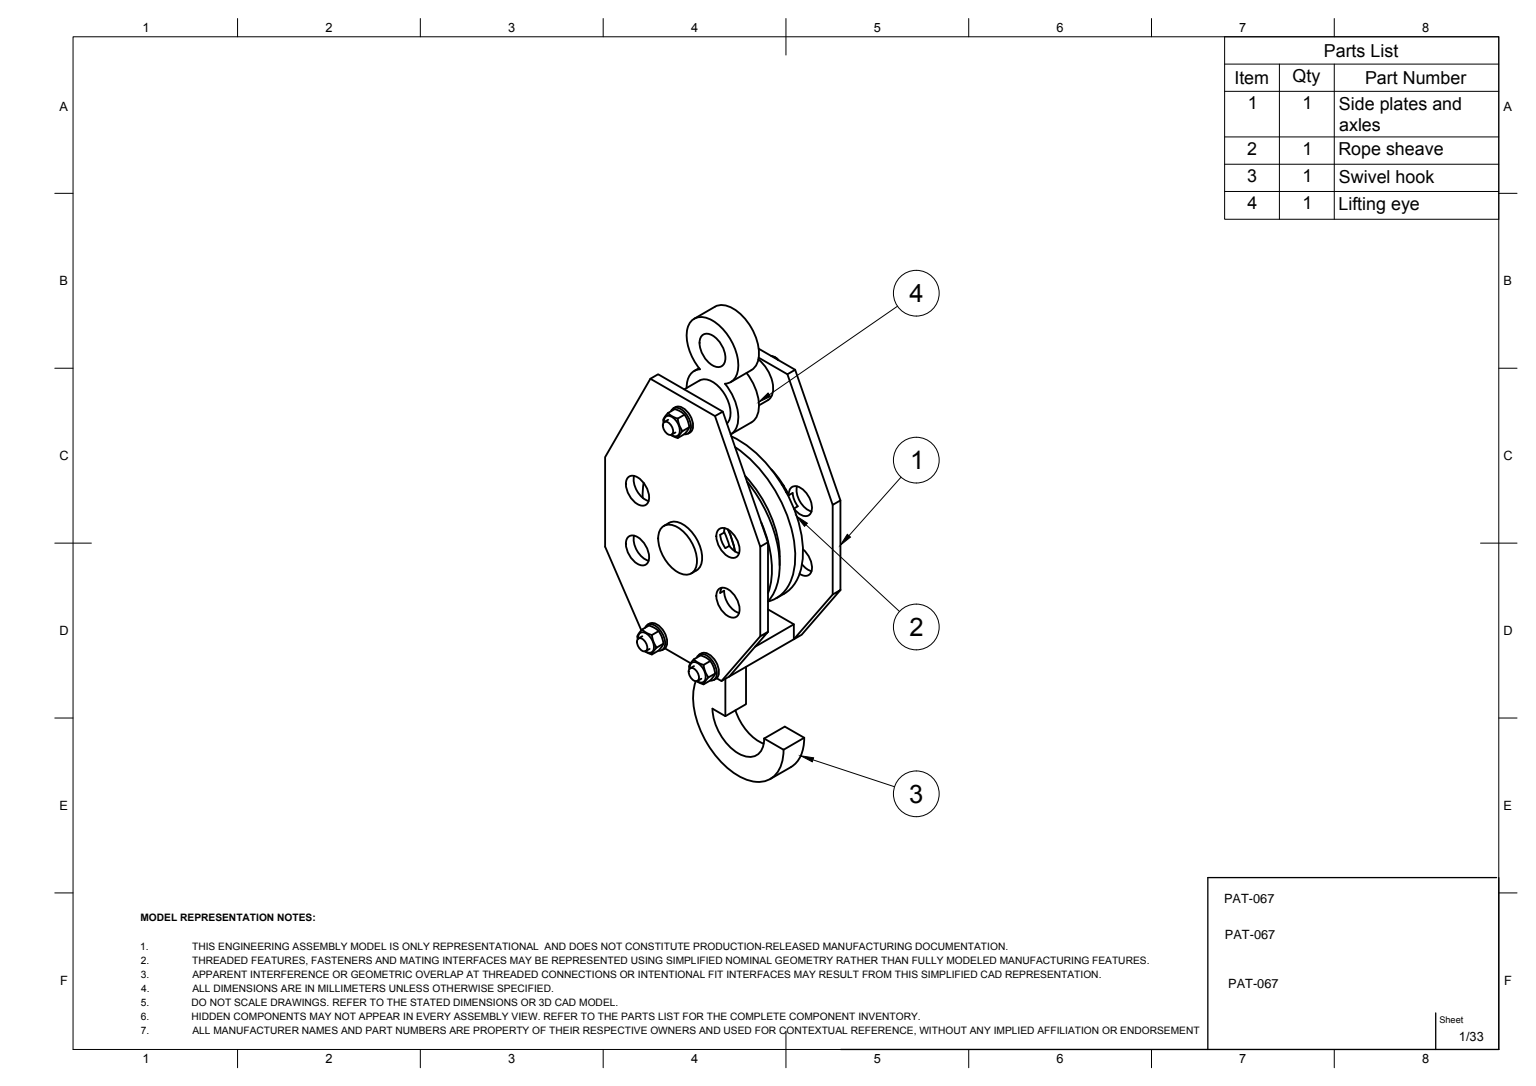
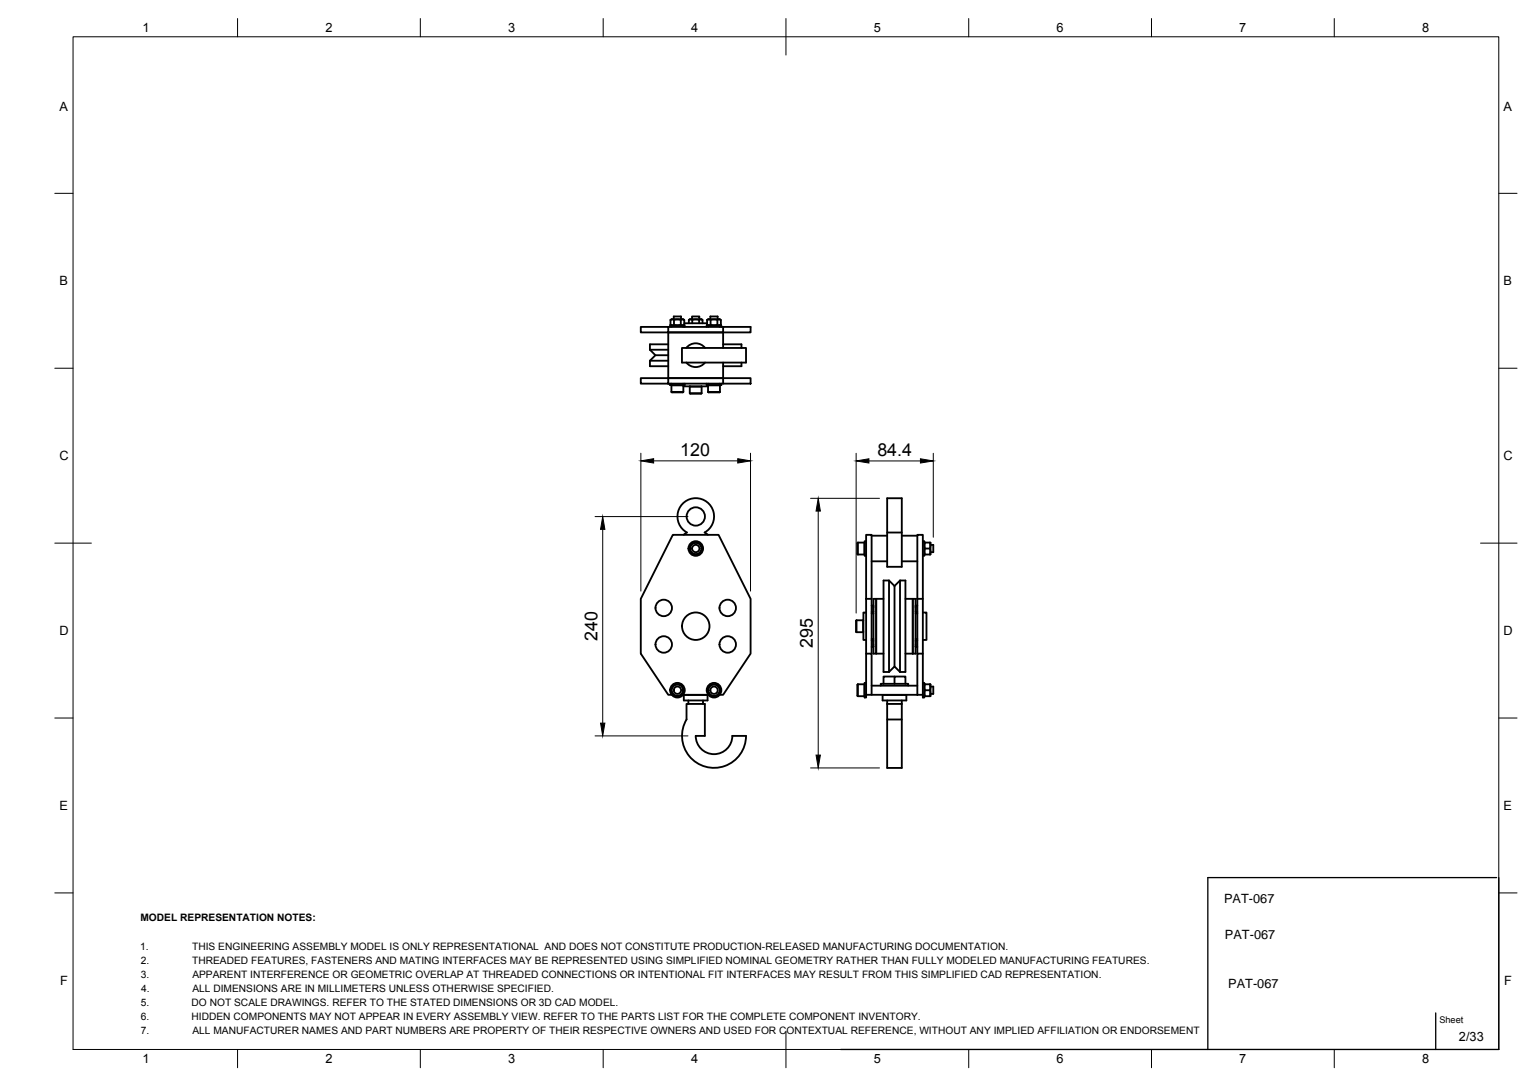
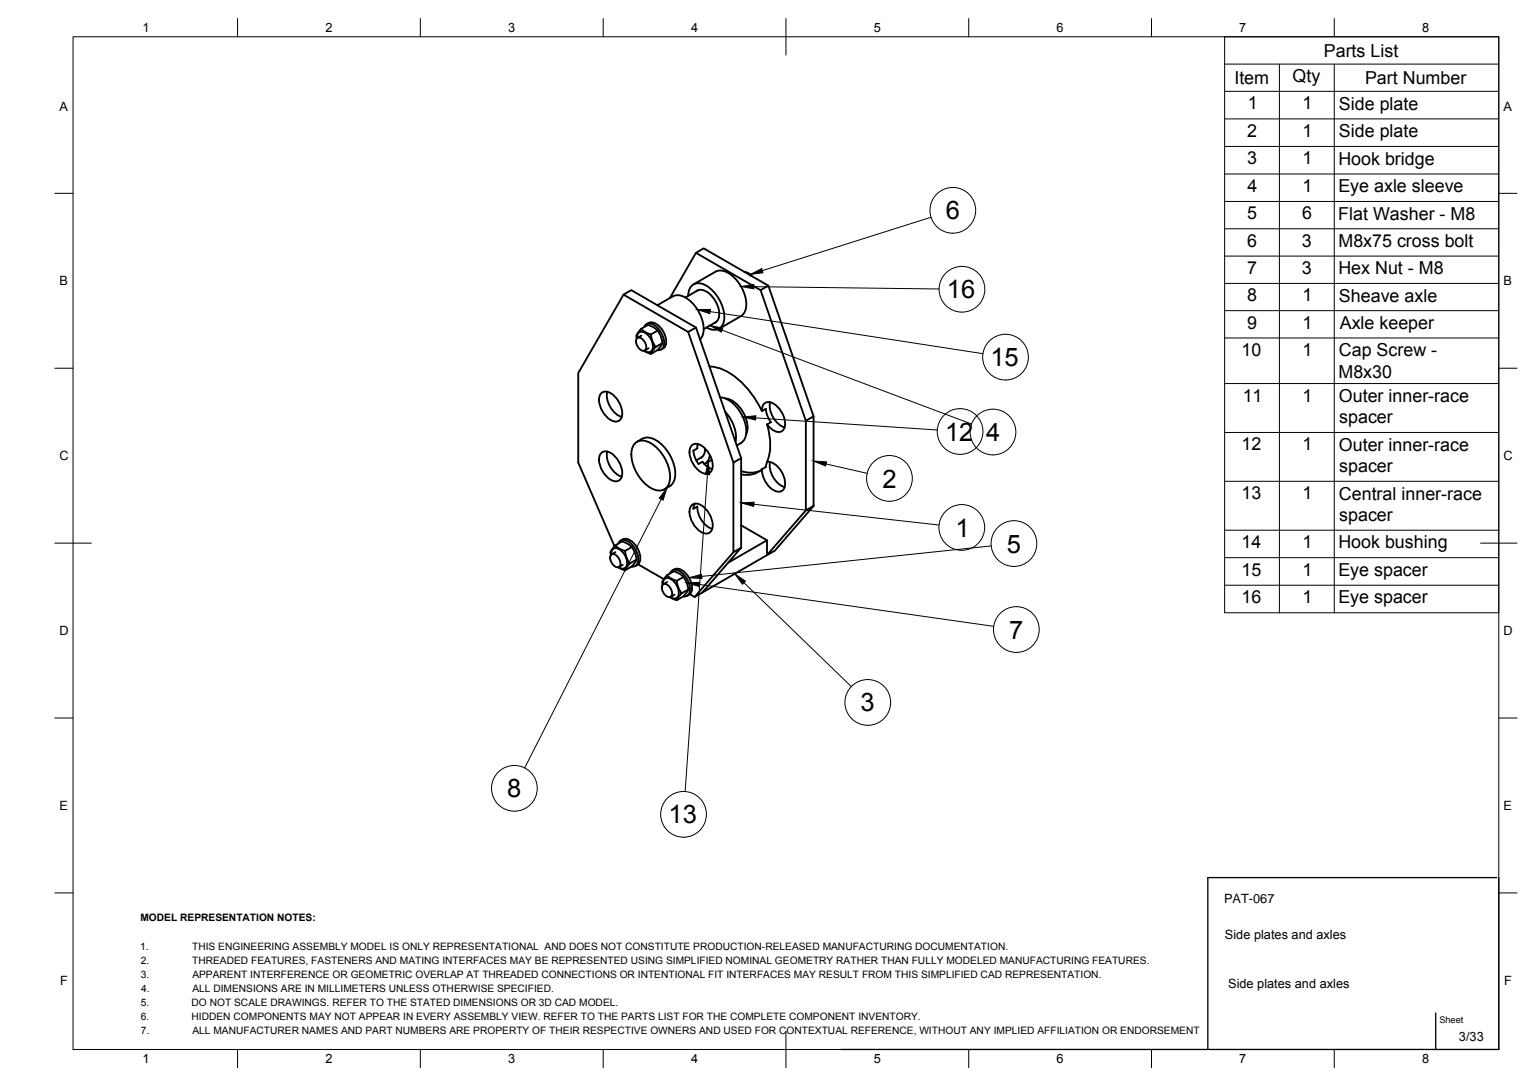
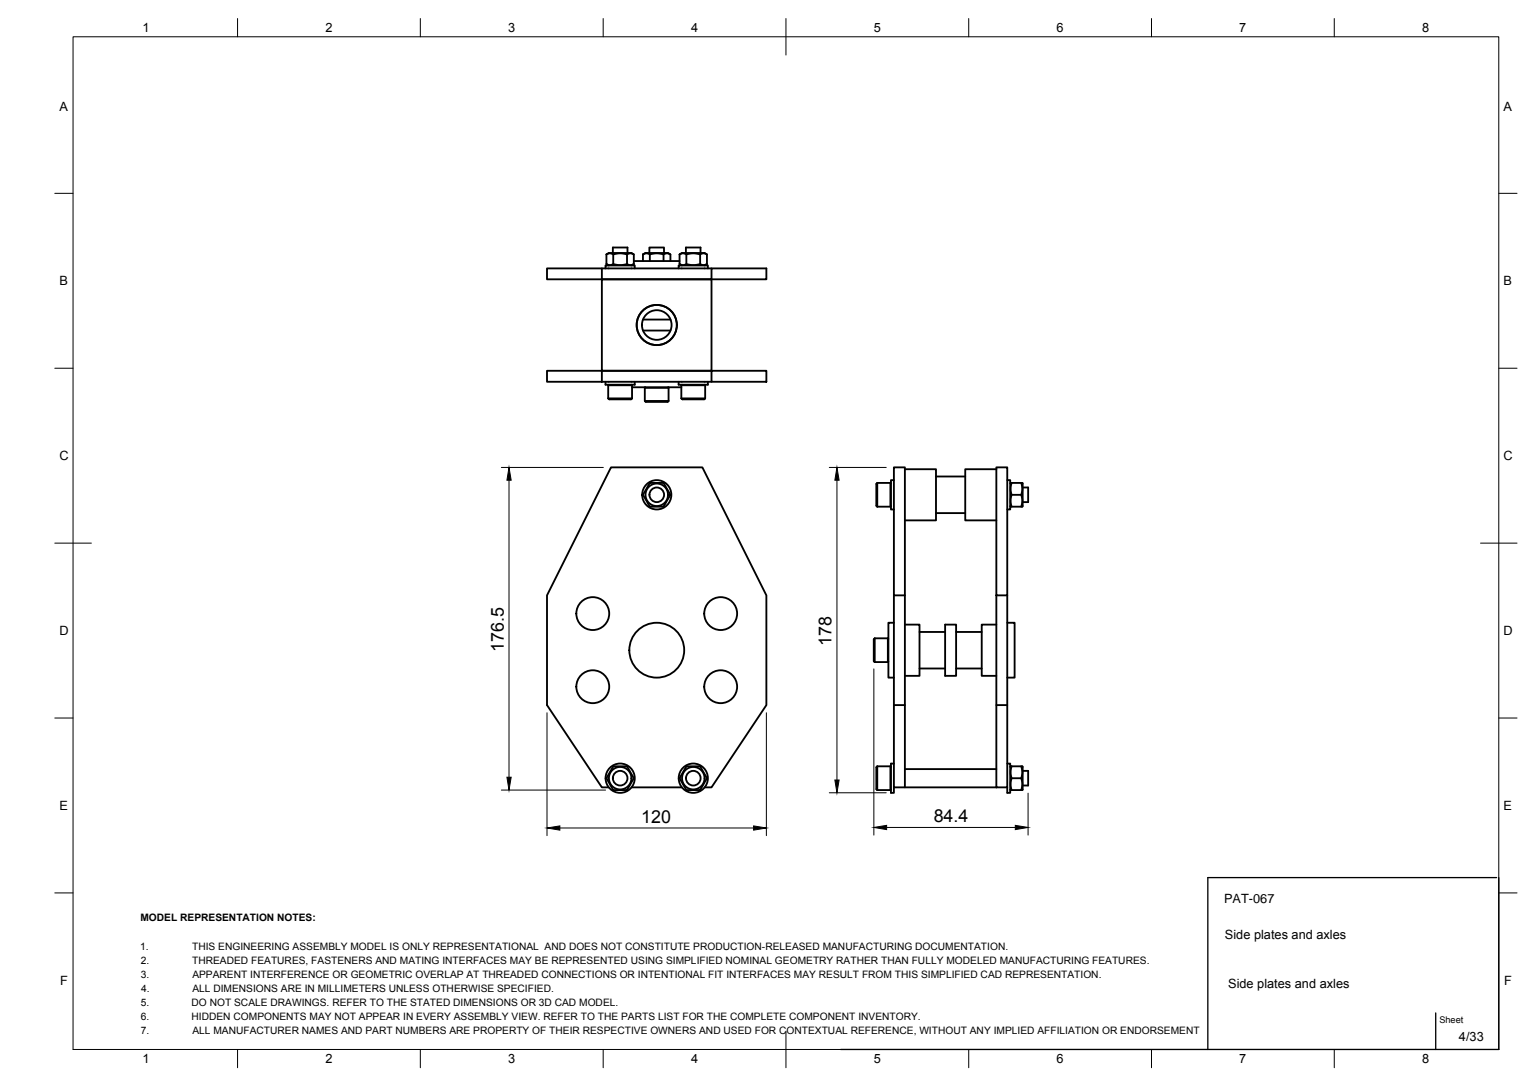
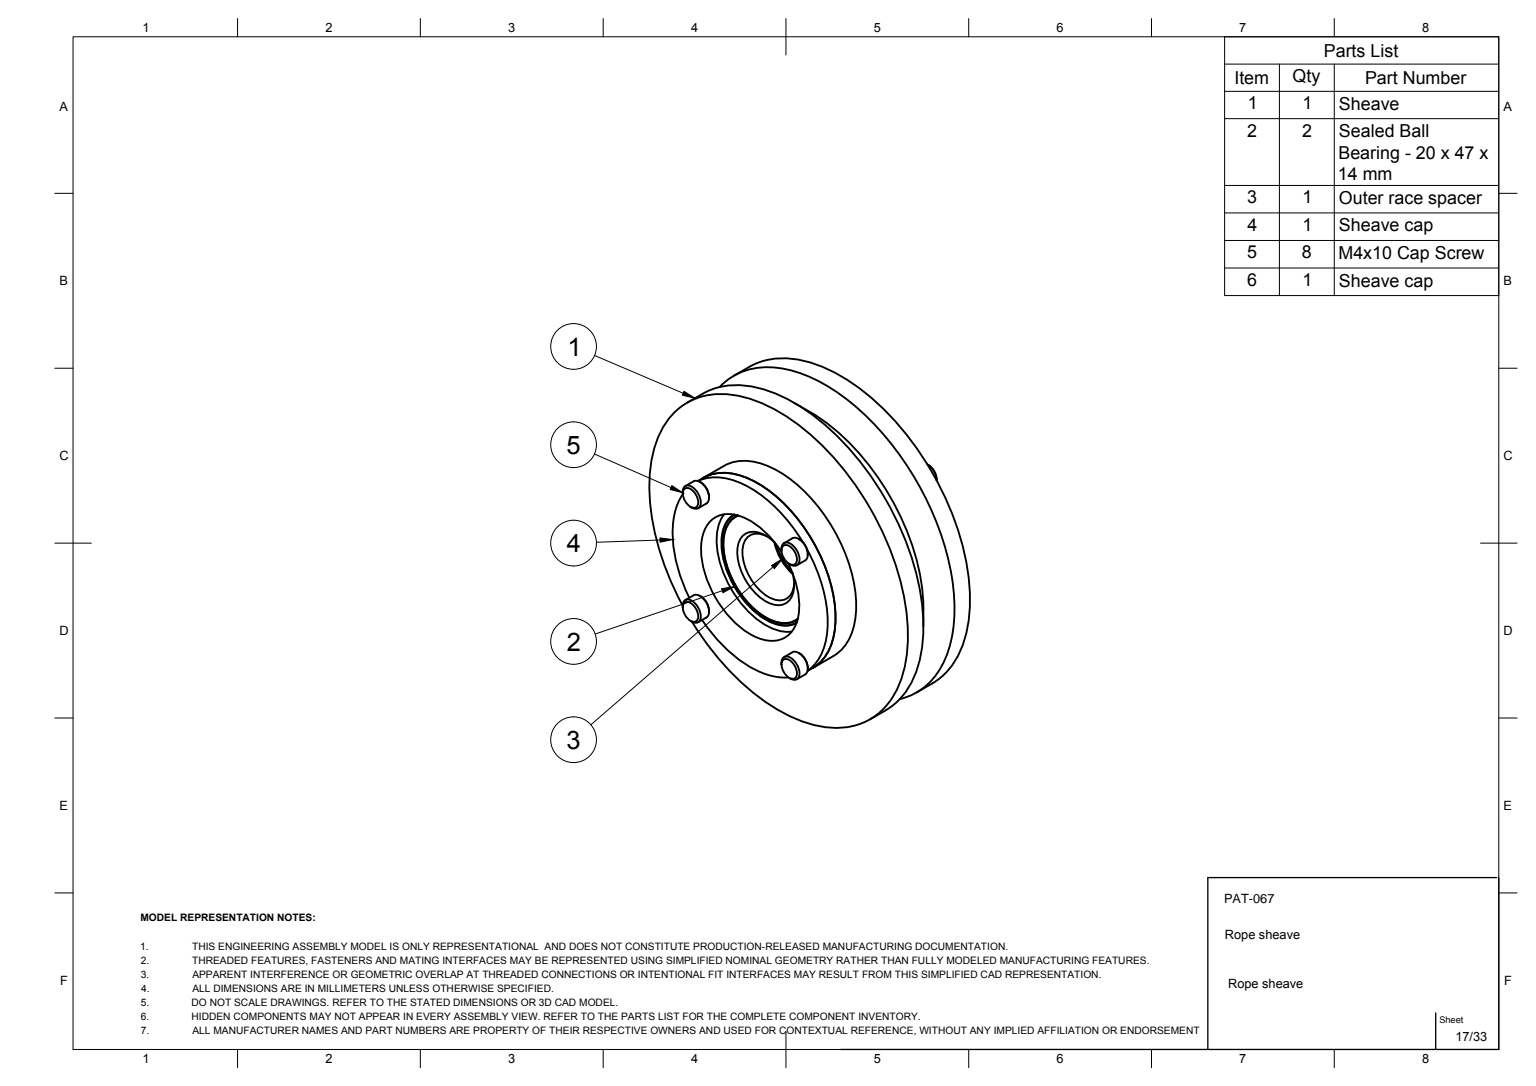
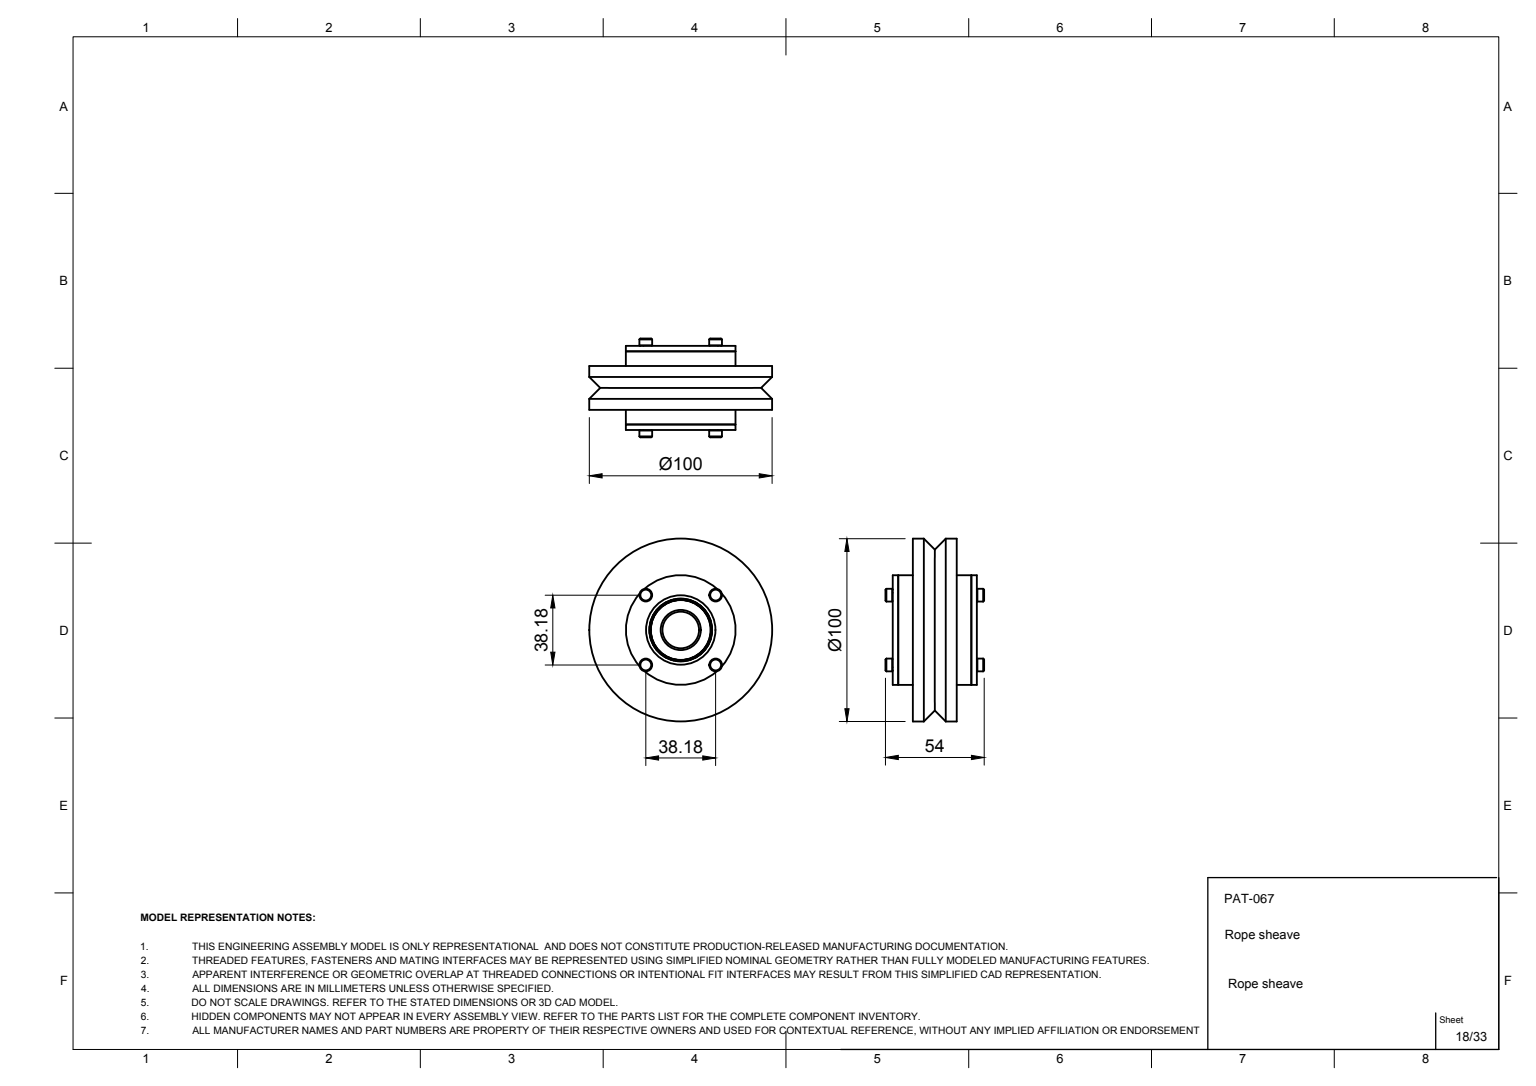
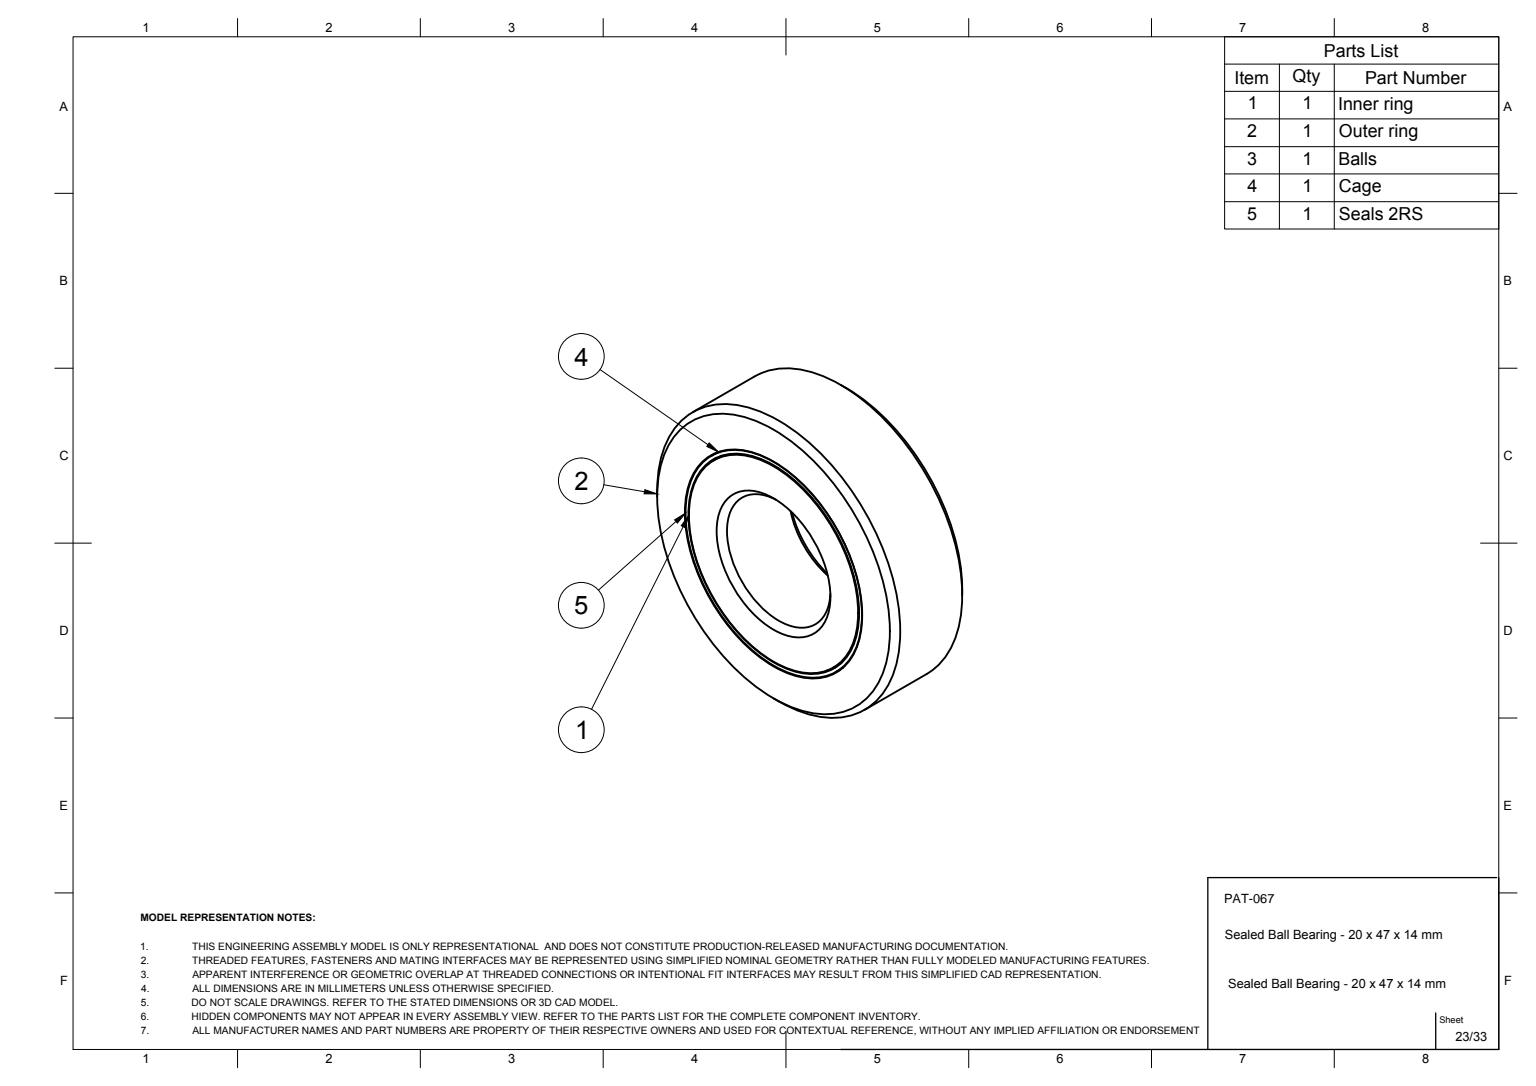
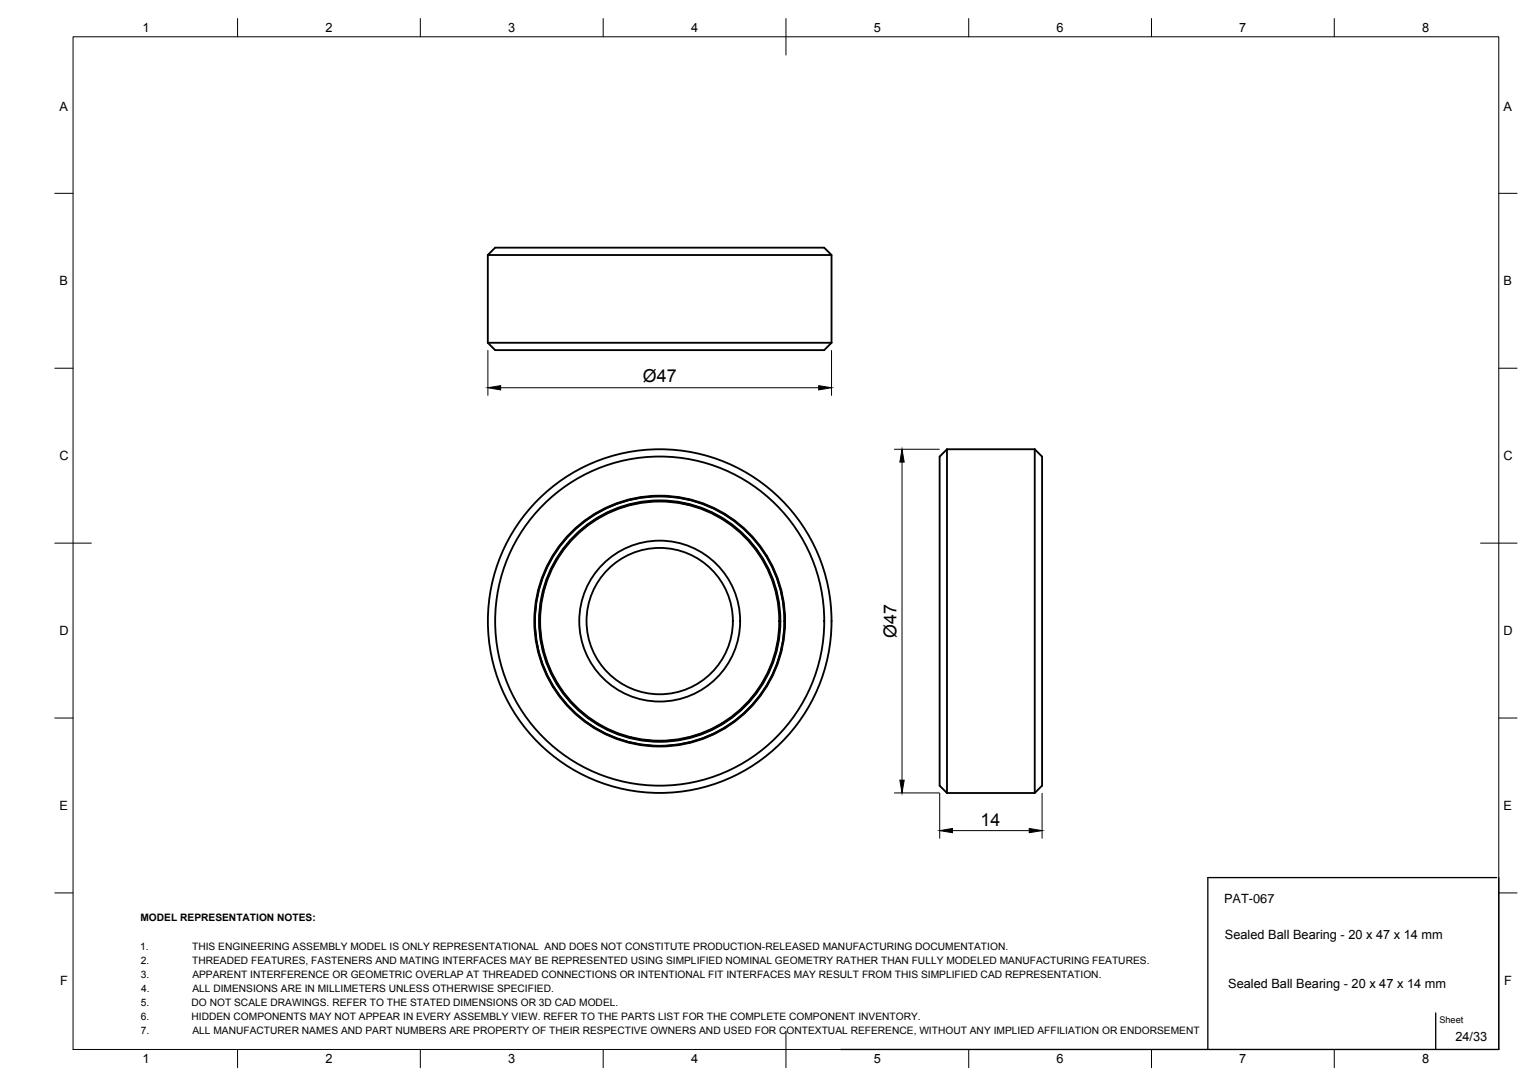
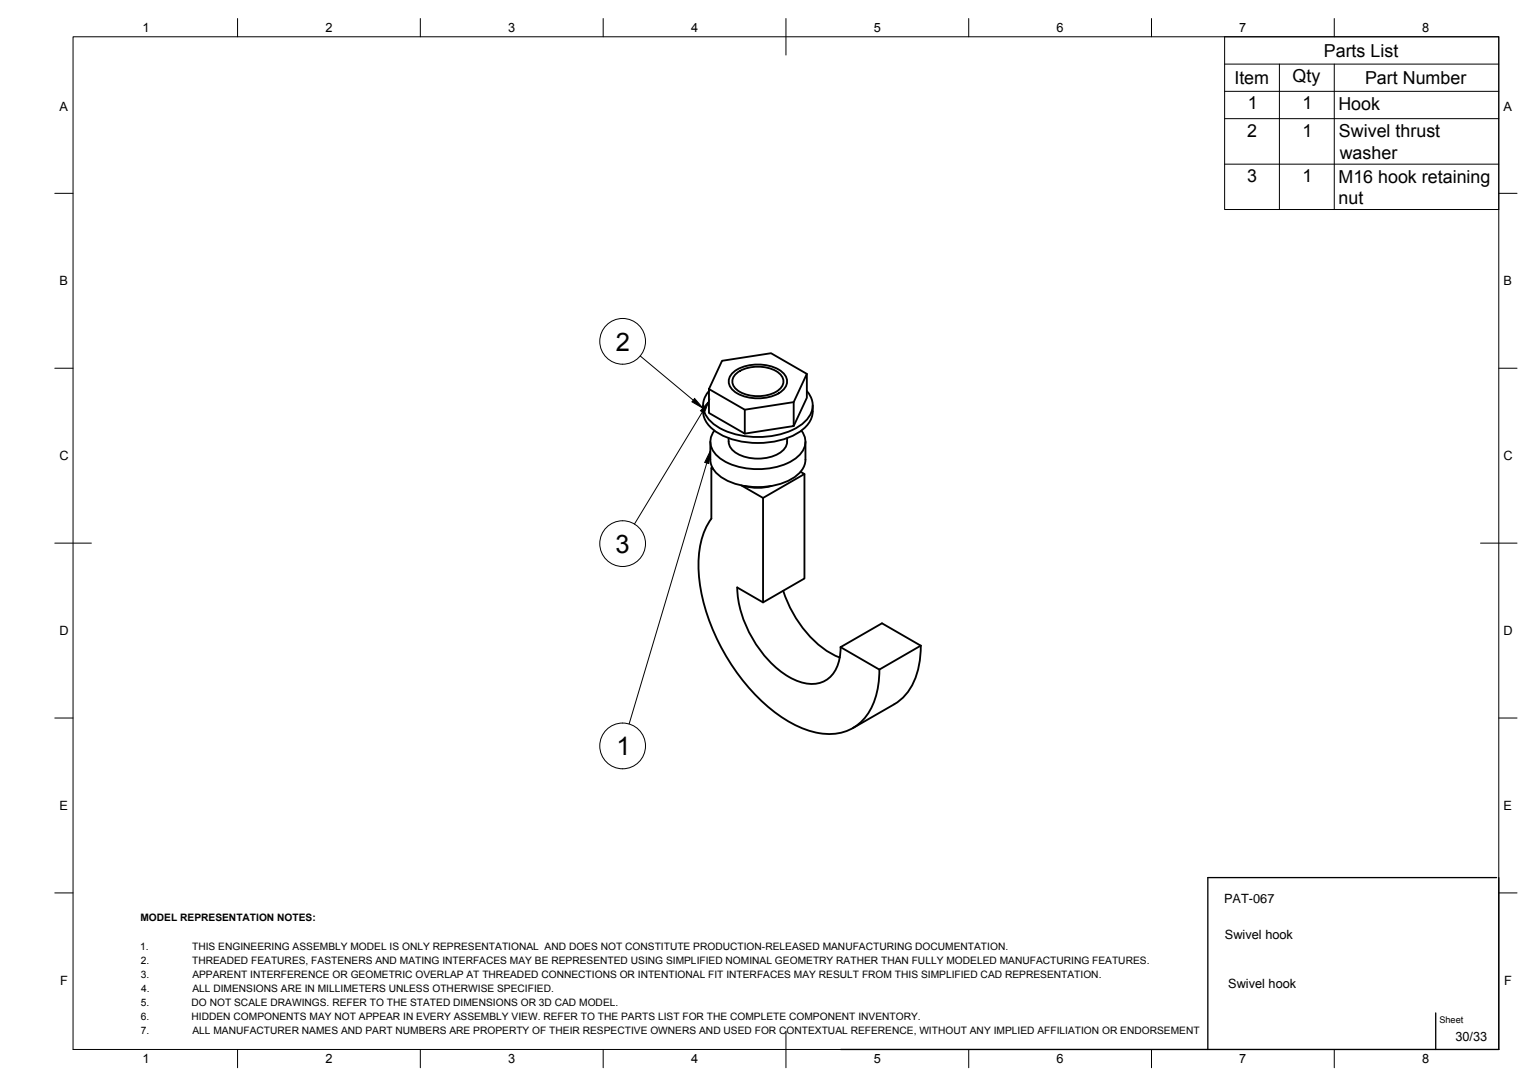
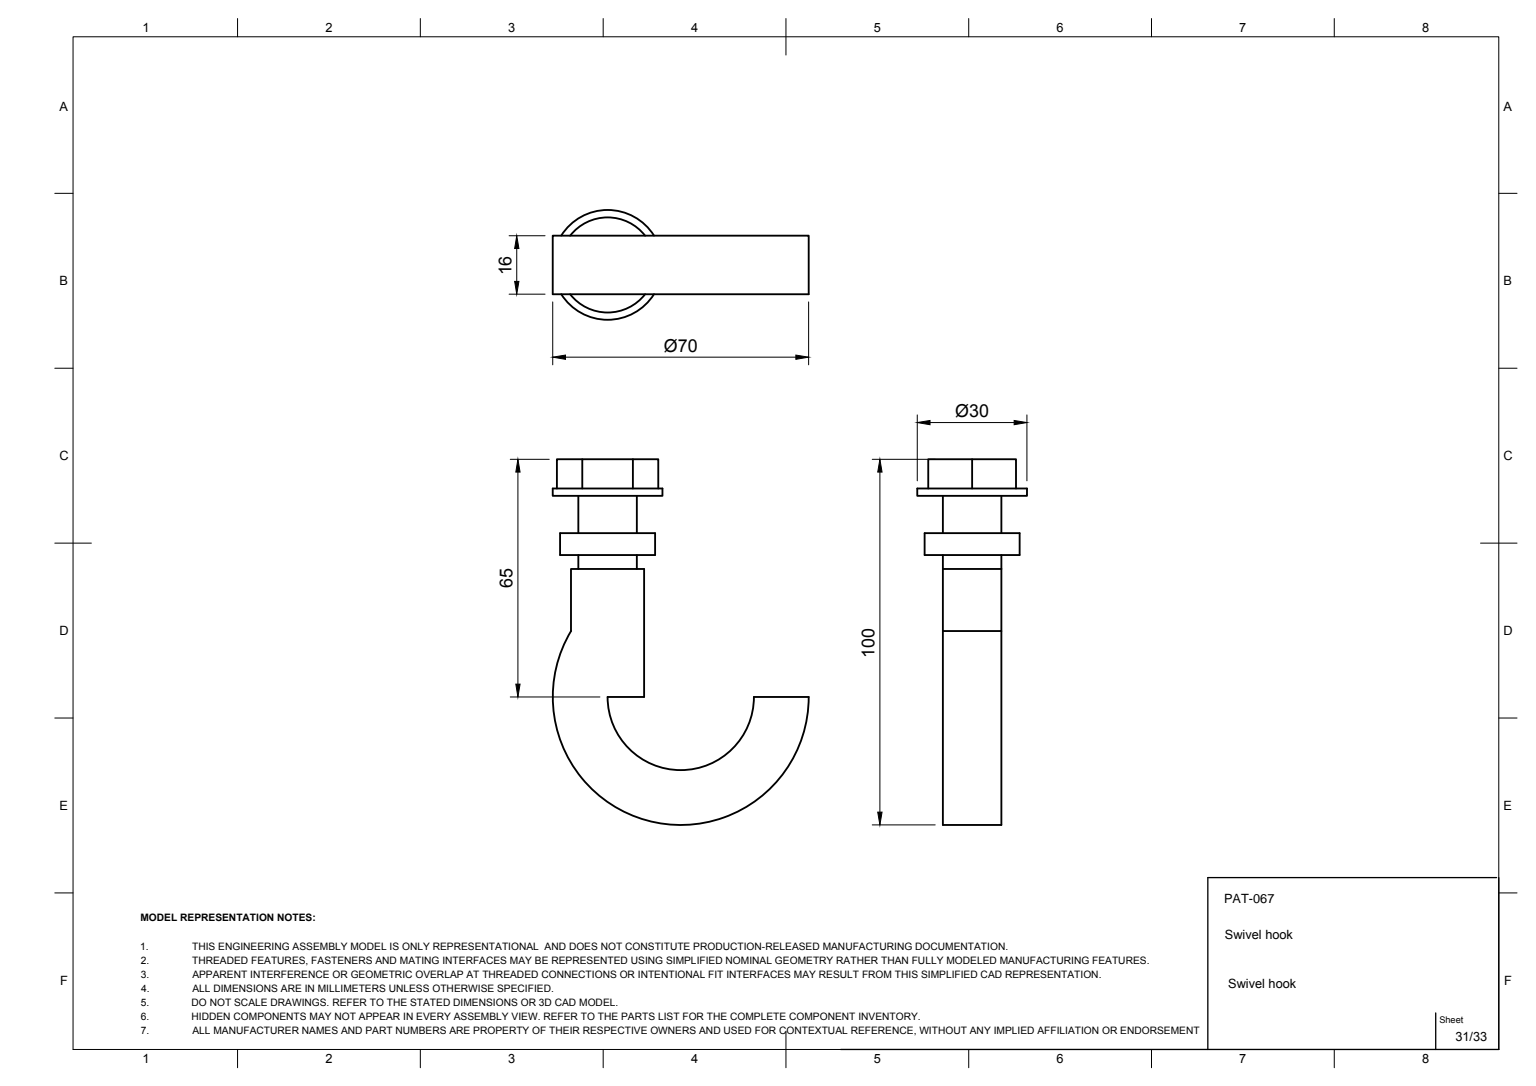
ISO-10303-21;
HEADER;
/* Generated by software containing ST-Developer
 * from STEP Tools, Inc. (www.steptools.com) 
 */

FILE_DESCRIPTION(
/* description */ ('Lifting hook block with sheave'),
/* implementation_level */ '2;1');

FILE_NAME(
/* name */ 'PAT-067',
/* time_stamp */ '2026-10-28T03:23:54-07:00',
/* author */ (''),
/* organization */ (''),
/* preprocessor_version */ 'ST-DEVELOPER v20.2',
/* originating_system */ 'Autodesk Translation Framework v15.17.0.0',
/* authorisation */ '');

FILE_SCHEMA (('AUTOMOTIVE_DESIGN { 1 0 10303 214 3 1 1 }'));
ENDSEC;

DATA;
#10=MECHANICAL_DESIGN_GEOMETRIC_PRESENTATION_REPRESENTATION('',(#351,#352,
#353,#354,#355,#356,#357,#358,#359,#360,#361,#362,#363,#364,#365,#366,#367,
#368,#369,#370,#371,#372,#373,#374,#375,#376,#377,#378,#379,#380,#381,#382,
#383,#384,#385,#386,#387,#388),#9391);
#11=B_SPLINE_CURVE_WITH_KNOTS('',3,(#8590,#8591,#8592,#8593,#8594,#8595,
#8596,#8597,#8598,#8599,#8600,#8601,#8602,#8603,#8604,#8605,#8606,#8607,
#8608,#8609,#8610,#8611),.UNSPECIFIED.,.F.,.F.,(4,2,2,2,2,2,2,2,2,2,4),
(0.0789094028588958,0.210573405340968,0.315860108011452,0.421146810681936,
0.522142632548711,0.623138454415485,0.72413427628226,0.825130098149035,
0.930416800819519,1.03570350349,1.16736750597208),.UNSPECIFIED.);
#12=B_SPLINE_CURVE_WITH_KNOTS('',3,(#8615,#8616,#8617,#8618,#8619,#8620,
#8621,#8622,#8623,#8624,#8625,#8626,#8627,#8628,#8629,#8630,#8631,#8632,
#8633,#8634,#8635,#8636),.UNSPECIFIED.,.F.,.F.,(4,2,2,2,2,2,2,2,2,2,4),
(0.0774793363974613,0.142088896491891,0.284177792983782,0.411119756996526,
0.514392970548519,0.617666184100513,0.720939397652506,0.8242126112045,0.951154575217244,
1.09324347170913,1.15785303180356),.UNSPECIFIED.);
#13=B_SPLINE_CURVE_WITH_KNOTS('',3,(#8642,#8643,#8644,#8645,#8646,#8647,
#8648,#8649,#8650,#8651,#8652,#8653,#8654,#8655,#8656,#8657,#8658,#8659,
#8660,#8661,#8662,#8663),.UNSPECIFIED.,.F.,.F.,(4,2,2,2,2,2,2,2,2,2,4),
(0.0774793363974613,0.142088896491891,0.284177792983782,0.411119756996525,
0.514392970548519,0.617666184100513,0.720939397652506,0.8242126112045,0.951154575217243,
1.09324347170913,1.15785303180356),.UNSPECIFIED.);
#14=B_SPLINE_CURVE_WITH_KNOTS('',3,(#8667,#8668,#8669,#8670,#8671,#8672,
#8673,#8674,#8675,#8676,#8677,#8678,#8679,#8680,#8681,#8682,#8683,#8684,
#8685,#8686,#8687,#8688),.UNSPECIFIED.,.F.,.F.,(4,2,2,2,2,2,2,2,2,2,4),
(0.0774793363974614,0.142088896491891,0.284177792983781,0.411119756996525,
0.514392970548519,0.617666184100512,0.720939397652506,0.824212611204499,
0.951154575217243,1.09324347170913,1.15785303180356),.UNSPECIFIED.);
#15=B_SPLINE_CURVE_WITH_KNOTS('',3,(#8692,#8693,#8694,#8695,#8696,#8697,
#8698,#8699,#8700,#8701,#8702,#8703),.UNSPECIFIED.,.F.,.F.,(4,2,2,2,2,4),
(0.0774793363974613,0.142088896491891,0.284177792983781,0.411119756996525,
0.514392970548519,0.617666184100512),.UNSPECIFIED.);
#16=B_SPLINE_CURVE_WITH_KNOTS('',3,(#8708,#8709,#8710,#8711,#8712,#8713,
#8714,#8715,#8716,#8717,#8718,#8719),.UNSPECIFIED.,.F.,.F.,(4,2,2,2,2,4),
(0.617666184100512,0.720939397652506,0.824212611204499,0.951154575217243,
1.09324347170913,1.15785303180356),.UNSPECIFIED.);
#17=B_SPLINE_CURVE_WITH_KNOTS('',3,(#8723,#8724,#8725,#8726,#8727,#8728,
#8729,#8730,#8731,#8732,#8733,#8734,#8735,#8736,#8737,#8738,#8739,#8740,
#8741,#8742,#8743,#8744),.UNSPECIFIED.,.F.,.F.,(4,2,2,2,2,2,2,2,2,2,4),
(0.0774793363974613,0.142088896491891,0.284177792983782,0.411119756996526,
0.514392970548519,0.617666184100513,0.720939397652507,0.8242126112045,0.951154575217245,
1.09324347170914,1.15785303180356),.UNSPECIFIED.);
#18=B_SPLINE_CURVE_WITH_KNOTS('',3,(#8748,#8749,#8750,#8751,#8752,#8753,
#8754,#8755,#8756,#8757,#8758,#8759,#8760,#8761,#8762,#8763,#8764,#8765,
#8766,#8767,#8768,#8769),.UNSPECIFIED.,.F.,.F.,(4,2,2,2,2,2,2,2,2,2,4),
(0.0774793363974613,0.142088896491891,0.284177792983782,0.411119756996526,
0.514392970548519,0.617666184100513,0.720939397652506,0.824212611204499,
0.951154575217243,1.09324347170913,1.15785303180356),.UNSPECIFIED.);
#19=B_SPLINE_CURVE_WITH_KNOTS('',3,(#8773,#8774,#8775,#8776,#8777,#8778,
#8779,#8780,#8781,#8782,#8783,#8784,#8785,#8786,#8787,#8788,#8789,#8790,
#8791,#8792,#8793,#8794),.UNSPECIFIED.,.F.,.F.,(4,2,2,2,2,2,2,2,2,2,4),
(0.0774793363974613,0.142088896491891,0.284177792983782,0.411119756996526,
0.514392970548519,0.617666184100513,0.720939397652506,0.8242126112045,0.951154575217244,
1.09324347170913,1.15785303180356),.UNSPECIFIED.);
#20=B_SPLINE_CURVE_WITH_KNOTS('',3,(#8798,#8799,#8800,#8801,#8802,#8803,
#8804,#8805,#8806,#8807,#8808,#8809,#8810,#8811,#8812,#8813,#8814,#8815,
#8816,#8817,#8818,#8819),.UNSPECIFIED.,.F.,.F.,(4,2,2,2,2,2,2,2,2,2,4),
(0.0774793363974613,0.142088896491891,0.284177792983782,0.411119756996526,
0.514392970548519,0.617666184100513,0.720939397652506,0.8242126112045,0.951154575217243,
1.09324347170913,1.15785303180356),.UNSPECIFIED.);
#21=B_SPLINE_CURVE_WITH_KNOTS('',3,(#8827,#8828,#8829,#8830,#8831,#8832,
#8833,#8834,#8835,#8836,#8837,#8838,#8839,#8840,#8841,#8842,#8843,#8844,
#8845,#8846,#8847,#8848),.UNSPECIFIED.,.F.,.F.,(4,2,2,2,2,2,2,2,2,2,4),
(0.0789094028588958,0.210573405340968,0.315860108011452,0.421146810681936,
0.522142632548711,0.623138454415485,0.72413427628226,0.825130098149035,
0.930416800819519,1.03570350349,1.16736750597208),.UNSPECIFIED.);
#22=B_SPLINE_CURVE_WITH_KNOTS('',3,(#8856,#8857,#8858,#8859,#8860,#8861,
#8862,#8863,#8864,#8865,#8866,#8867,#8868,#8869,#8870,#8871,#8872,#8873,
#8874,#8875,#8876,#8877),.UNSPECIFIED.,.F.,.F.,(4,2,2,2,2,2,2,2,2,2,4),
(0.0789094028588958,0.210573405340969,0.315860108011453,0.421146810681937,
0.522142632548712,0.623138454415486,0.724134276282261,0.825130098149035,
0.930416800819519,1.03570350349,1.16736750597208),.UNSPECIFIED.);
#23=B_SPLINE_CURVE_WITH_KNOTS('',3,(#8886,#8887,#8888,#8889,#8890,#8891,
#8892,#8893,#8894,#8895,#8896,#8897),.UNSPECIFIED.,.F.,.F.,(4,2,2,2,2,4),
(0.0789094028588958,0.210573405340968,0.315860108011452,0.421146810681937,
0.522142632548711,0.623138454415486),.UNSPECIFIED.);
#24=B_SPLINE_CURVE_WITH_KNOTS('',3,(#8899,#8900,#8901,#8902,#8903,#8904,
#8905,#8906,#8907,#8908,#8909,#8910),.UNSPECIFIED.,.F.,.F.,(4,2,2,2,2,4),
(0.623138454415486,0.72413427628226,0.825130098149035,0.930416800819519,
1.03570350349,1.16736750597208),.UNSPECIFIED.);
#25=B_SPLINE_CURVE_WITH_KNOTS('',3,(#8917,#8918,#8919,#8920,#8921,#8922,
#8923,#8924,#8925,#8926,#8927,#8928,#8929,#8930,#8931,#8932,#8933,#8934,
#8935,#8936,#8937,#8938),.UNSPECIFIED.,.F.,.F.,(4,2,2,2,2,2,2,2,2,2,4),
(0.0789094028588958,0.210573405340968,0.315860108011452,0.421146810681936,
0.522142632548711,0.623138454415486,0.72413427628226,0.825130098149035,
0.930416800819519,1.03570350349,1.16736750597208),.UNSPECIFIED.);
#26=B_SPLINE_CURVE_WITH_KNOTS('',3,(#8946,#8947,#8948,#8949,#8950,#8951,
#8952,#8953,#8954,#8955,#8956,#8957,#8958,#8959,#8960,#8961,#8962,#8963,
#8964,#8965,#8966,#8967),.UNSPECIFIED.,.F.,.F.,(4,2,2,2,2,2,2,2,2,2,4),
(0.0789094028588957,0.210573405340968,0.315860108011452,0.421146810681936,
0.522142632548711,0.623138454415485,0.72413427628226,0.825130098149035,
0.930416800819519,1.03570350349,1.16736750597207),.UNSPECIFIED.);
#27=B_SPLINE_CURVE_WITH_KNOTS('',3,(#8975,#8976,#8977,#8978,#8979,#8980,
#8981,#8982,#8983,#8984,#8985,#8986,#8987,#8988,#8989,#8990,#8991,#8992,
#8993,#8994,#8995,#8996),.UNSPECIFIED.,.F.,.F.,(4,2,2,2,2,2,2,2,2,2,4),
(0.0789094028588958,0.210573405340968,0.315860108011452,0.421146810681936,
0.522142632548711,0.623138454415486,0.72413427628226,0.825130098149035,
0.930416800819519,1.03570350349,1.16736750597208),.UNSPECIFIED.);
#28=B_SPLINE_CURVE_WITH_KNOTS('',3,(#9005,#9006,#9007,#9008,#9009,#9010,
#9011,#9012,#9013,#9014,#9015,#9016,#9017,#9018,#9019,#9020,#9021,#9022,
#9023,#9024,#9025,#9026),.UNSPECIFIED.,.F.,.F.,(4,2,2,2,2,2,2,2,2,2,4),
(0.0789094028588958,0.210573405340968,0.315860108011452,0.421146810681936,
0.522142632548711,0.623138454415485,0.72413427628226,0.825130098149035,
0.930416800819519,1.03570350349,1.16736750597208),.UNSPECIFIED.);
#29=SPHERICAL_SURFACE('',#5724,0.3969);
#30=SPHERICAL_SURFACE('',#5726,0.3969);
#31=SPHERICAL_SURFACE('',#5728,0.3969);
#32=SPHERICAL_SURFACE('',#5730,0.3969);
#33=SPHERICAL_SURFACE('',#5732,0.3969);
#34=SPHERICAL_SURFACE('',#5734,0.3969);
#35=SPHERICAL_SURFACE('',#5736,0.3969);
#36=SPHERICAL_SURFACE('',#5738,0.3969);
#37=SPHERICAL_SURFACE('',#5741,0.412776);
#38=SPHERICAL_SURFACE('',#5757,0.412776);
#39=SPHERICAL_SURFACE('',#5762,0.412776);
#40=SPHERICAL_SURFACE('',#5767,0.412776);
#41=SPHERICAL_SURFACE('',#5772,0.412776);
#42=SPHERICAL_SURFACE('',#5777,0.412776);
#43=SPHERICAL_SURFACE('',#5782,0.412776);
#44=SPHERICAL_SURFACE('',#5790,0.412776);
#45=TOROIDAL_SURFACE('',#5684,1.675,0.412776);
#46=TOROIDAL_SURFACE('',#5704,1.675,0.412776);
#47=ITEM_DEFINED_TRANSFORMATION($,$,#5261,#5562);
#48=ITEM_DEFINED_TRANSFORMATION($,$,#5321,#5563);
#49=ITEM_DEFINED_TRANSFORMATION($,$,#5381,#5564);
#50=ITEM_DEFINED_TRANSFORMATION($,$,#5397,#5565);
#51=ITEM_DEFINED_TRANSFORMATION($,$,#5406,#5566);
#52=ITEM_DEFINED_TRANSFORMATION($,$,#5420,#5567);
#53=ITEM_DEFINED_TRANSFORMATION($,$,#5429,#5568);
#54=ITEM_DEFINED_TRANSFORMATION($,$,#5438,#5569);
#55=ITEM_DEFINED_TRANSFORMATION($,$,#5447,#5570);
#56=ITEM_DEFINED_TRANSFORMATION($,$,#5456,#5571);
#57=ITEM_DEFINED_TRANSFORMATION($,$,#5465,#5572);
#58=ITEM_DEFINED_TRANSFORMATION($,$,#5474,#5573);
#59=ITEM_DEFINED_TRANSFORMATION($,$,#5511,#5574);
#60=ITEM_DEFINED_TRANSFORMATION($,$,#5483,#5575);
#61=ITEM_DEFINED_TRANSFORMATION($,$,#5511,#5576);
#62=ITEM_DEFINED_TRANSFORMATION($,$,#5520,#5577);
#63=ITEM_DEFINED_TRANSFORMATION($,$,#5511,#5578);
#64=ITEM_DEFINED_TRANSFORMATION($,$,#5483,#5579);
#65=ITEM_DEFINED_TRANSFORMATION($,$,#5511,#5580);
#66=ITEM_DEFINED_TRANSFORMATION($,$,#5520,#5581);
#67=ITEM_DEFINED_TRANSFORMATION($,$,#5511,#5582);
#68=ITEM_DEFINED_TRANSFORMATION($,$,#5483,#5583);
#69=ITEM_DEFINED_TRANSFORMATION($,$,#5511,#5584);
#70=ITEM_DEFINED_TRANSFORMATION($,$,#5520,#5585);
#71=ITEM_DEFINED_TRANSFORMATION($,$,#5536,#5586);
#72=ITEM_DEFINED_TRANSFORMATION($,$,#5683,#5811);
#73=ITEM_DEFINED_TRANSFORMATION($,$,#5703,#5812);
#74=ITEM_DEFINED_TRANSFORMATION($,$,#5723,#5813);
#75=ITEM_DEFINED_TRANSFORMATION($,$,#5740,#5814);
#76=ITEM_DEFINED_TRANSFORMATION($,$,#5794,#5815);
#77=ITEM_DEFINED_TRANSFORMATION($,$,#5588,#5840);
#78=ITEM_DEFINED_TRANSFORMATION($,$,#5623,#5841);
#79=ITEM_DEFINED_TRANSFORMATION($,$,#5632,#5842);
#80=ITEM_DEFINED_TRANSFORMATION($,$,#5657,#5843);
#81=ITEM_DEFINED_TRANSFORMATION($,$,#5682,#5844);
#82=ITEM_DEFINED_TRANSFORMATION($,$,#5682,#5845);
#83=ITEM_DEFINED_TRANSFORMATION($,$,#5816,#5846);
#84=ITEM_DEFINED_TRANSFORMATION($,$,#5816,#5847);
#85=ITEM_DEFINED_TRANSFORMATION($,$,#5816,#5848);
#86=ITEM_DEFINED_TRANSFORMATION($,$,#5816,#5849);
#87=ITEM_DEFINED_TRANSFORMATION($,$,#5816,#5850);
#88=ITEM_DEFINED_TRANSFORMATION($,$,#5816,#5851);
#89=ITEM_DEFINED_TRANSFORMATION($,$,#5816,#5852);
#90=ITEM_DEFINED_TRANSFORMATION($,$,#5816,#5853);
#91=ITEM_DEFINED_TRANSFORMATION($,$,#5855,#5905);
#92=ITEM_DEFINED_TRANSFORMATION($,$,#5884,#5906);
#93=ITEM_DEFINED_TRANSFORMATION($,$,#5893,#5907);
#94=ITEM_DEFINED_TRANSFORMATION($,$,#5909,#5924);
#95=ITEM_DEFINED_TRANSFORMATION($,$,#5260,#5925);
#96=ITEM_DEFINED_TRANSFORMATION($,$,#5587,#5926);
#97=ITEM_DEFINED_TRANSFORMATION($,$,#5854,#5927);
#98=ITEM_DEFINED_TRANSFORMATION($,$,#5908,#5928);
#99=(
REPRESENTATION_RELATIONSHIP($,$,#9522,#9521)
REPRESENTATION_RELATIONSHIP_WITH_TRANSFORMATION(#47)
SHAPE_REPRESENTATION_RELATIONSHIP()
);
#100=(
REPRESENTATION_RELATIONSHIP($,$,#9523,#9521)
REPRESENTATION_RELATIONSHIP_WITH_TRANSFORMATION(#48)
SHAPE_REPRESENTATION_RELATIONSHIP()
);
#101=(
REPRESENTATION_RELATIONSHIP($,$,#9524,#9521)
REPRESENTATION_RELATIONSHIP_WITH_TRANSFORMATION(#49)
SHAPE_REPRESENTATION_RELATIONSHIP()
);
#102=(
REPRESENTATION_RELATIONSHIP($,$,#9525,#9521)
REPRESENTATION_RELATIONSHIP_WITH_TRANSFORMATION(#50)
SHAPE_REPRESENTATION_RELATIONSHIP()
);
#103=(
REPRESENTATION_RELATIONSHIP($,$,#9526,#9521)
REPRESENTATION_RELATIONSHIP_WITH_TRANSFORMATION(#51)
SHAPE_REPRESENTATION_RELATIONSHIP()
);
#104=(
REPRESENTATION_RELATIONSHIP($,$,#9527,#9521)
REPRESENTATION_RELATIONSHIP_WITH_TRANSFORMATION(#52)
SHAPE_REPRESENTATION_RELATIONSHIP()
);
#105=(
REPRESENTATION_RELATIONSHIP($,$,#9528,#9521)
REPRESENTATION_RELATIONSHIP_WITH_TRANSFORMATION(#53)
SHAPE_REPRESENTATION_RELATIONSHIP()
);
#106=(
REPRESENTATION_RELATIONSHIP($,$,#9529,#9521)
REPRESENTATION_RELATIONSHIP_WITH_TRANSFORMATION(#54)
SHAPE_REPRESENTATION_RELATIONSHIP()
);
#107=(
REPRESENTATION_RELATIONSHIP($,$,#9530,#9521)
REPRESENTATION_RELATIONSHIP_WITH_TRANSFORMATION(#55)
SHAPE_REPRESENTATION_RELATIONSHIP()
);
#108=(
REPRESENTATION_RELATIONSHIP($,$,#9531,#9521)
REPRESENTATION_RELATIONSHIP_WITH_TRANSFORMATION(#56)
SHAPE_REPRESENTATION_RELATIONSHIP()
);
#109=(
REPRESENTATION_RELATIONSHIP($,$,#9532,#9521)
REPRESENTATION_RELATIONSHIP_WITH_TRANSFORMATION(#57)
SHAPE_REPRESENTATION_RELATIONSHIP()
);
#110=(
REPRESENTATION_RELATIONSHIP($,$,#9533,#9521)
REPRESENTATION_RELATIONSHIP_WITH_TRANSFORMATION(#58)
SHAPE_REPRESENTATION_RELATIONSHIP()
);
#111=(
REPRESENTATION_RELATIONSHIP($,$,#9535,#9521)
REPRESENTATION_RELATIONSHIP_WITH_TRANSFORMATION(#59)
SHAPE_REPRESENTATION_RELATIONSHIP()
);
#112=(
REPRESENTATION_RELATIONSHIP($,$,#9534,#9521)
REPRESENTATION_RELATIONSHIP_WITH_TRANSFORMATION(#60)
SHAPE_REPRESENTATION_RELATIONSHIP()
);
#113=(
REPRESENTATION_RELATIONSHIP($,$,#9535,#9521)
REPRESENTATION_RELATIONSHIP_WITH_TRANSFORMATION(#61)
SHAPE_REPRESENTATION_RELATIONSHIP()
);
#114=(
REPRESENTATION_RELATIONSHIP($,$,#9536,#9521)
REPRESENTATION_RELATIONSHIP_WITH_TRANSFORMATION(#62)
SHAPE_REPRESENTATION_RELATIONSHIP()
);
#115=(
REPRESENTATION_RELATIONSHIP($,$,#9535,#9521)
REPRESENTATION_RELATIONSHIP_WITH_TRANSFORMATION(#63)
SHAPE_REPRESENTATION_RELATIONSHIP()
);
#116=(
REPRESENTATION_RELATIONSHIP($,$,#9534,#9521)
REPRESENTATION_RELATIONSHIP_WITH_TRANSFORMATION(#64)
SHAPE_REPRESENTATION_RELATIONSHIP()
);
#117=(
REPRESENTATION_RELATIONSHIP($,$,#9535,#9521)
REPRESENTATION_RELATIONSHIP_WITH_TRANSFORMATION(#65)
SHAPE_REPRESENTATION_RELATIONSHIP()
);
#118=(
REPRESENTATION_RELATIONSHIP($,$,#9536,#9521)
REPRESENTATION_RELATIONSHIP_WITH_TRANSFORMATION(#66)
SHAPE_REPRESENTATION_RELATIONSHIP()
);
#119=(
REPRESENTATION_RELATIONSHIP($,$,#9535,#9521)
REPRESENTATION_RELATIONSHIP_WITH_TRANSFORMATION(#67)
SHAPE_REPRESENTATION_RELATIONSHIP()
);
#120=(
REPRESENTATION_RELATIONSHIP($,$,#9534,#9521)
REPRESENTATION_RELATIONSHIP_WITH_TRANSFORMATION(#68)
SHAPE_REPRESENTATION_RELATIONSHIP()
);
#121=(
REPRESENTATION_RELATIONSHIP($,$,#9535,#9521)
REPRESENTATION_RELATIONSHIP_WITH_TRANSFORMATION(#69)
SHAPE_REPRESENTATION_RELATIONSHIP()
);
#122=(
REPRESENTATION_RELATIONSHIP($,$,#9536,#9521)
REPRESENTATION_RELATIONSHIP_WITH_TRANSFORMATION(#70)
SHAPE_REPRESENTATION_RELATIONSHIP()
);
#123=(
REPRESENTATION_RELATIONSHIP($,$,#9537,#9521)
REPRESENTATION_RELATIONSHIP_WITH_TRANSFORMATION(#71)
SHAPE_REPRESENTATION_RELATIONSHIP()
);
#124=(
REPRESENTATION_RELATIONSHIP($,$,#9544,#9543)
REPRESENTATION_RELATIONSHIP_WITH_TRANSFORMATION(#72)
SHAPE_REPRESENTATION_RELATIONSHIP()
);
#125=(
REPRESENTATION_RELATIONSHIP($,$,#9545,#9543)
REPRESENTATION_RELATIONSHIP_WITH_TRANSFORMATION(#73)
SHAPE_REPRESENTATION_RELATIONSHIP()
);
#126=(
REPRESENTATION_RELATIONSHIP($,$,#9546,#9543)
REPRESENTATION_RELATIONSHIP_WITH_TRANSFORMATION(#74)
SHAPE_REPRESENTATION_RELATIONSHIP()
);
#127=(
REPRESENTATION_RELATIONSHIP($,$,#9547,#9543)
REPRESENTATION_RELATIONSHIP_WITH_TRANSFORMATION(#75)
SHAPE_REPRESENTATION_RELATIONSHIP()
);
#128=(
REPRESENTATION_RELATIONSHIP($,$,#9548,#9543)
REPRESENTATION_RELATIONSHIP_WITH_TRANSFORMATION(#76)
SHAPE_REPRESENTATION_RELATIONSHIP()
);
#129=(
REPRESENTATION_RELATIONSHIP($,$,#9539,#9538)
REPRESENTATION_RELATIONSHIP_WITH_TRANSFORMATION(#77)
SHAPE_REPRESENTATION_RELATIONSHIP()
);
#130=(
REPRESENTATION_RELATIONSHIP($,$,#9540,#9538)
REPRESENTATION_RELATIONSHIP_WITH_TRANSFORMATION(#78)
SHAPE_REPRESENTATION_RELATIONSHIP()
);
#131=(
REPRESENTATION_RELATIONSHIP($,$,#9541,#9538)
REPRESENTATION_RELATIONSHIP_WITH_TRANSFORMATION(#79)
SHAPE_REPRESENTATION_RELATIONSHIP()
);
#132=(
REPRESENTATION_RELATIONSHIP($,$,#9542,#9538)
REPRESENTATION_RELATIONSHIP_WITH_TRANSFORMATION(#80)
SHAPE_REPRESENTATION_RELATIONSHIP()
);
#133=(
REPRESENTATION_RELATIONSHIP($,$,#9543,#9538)
REPRESENTATION_RELATIONSHIP_WITH_TRANSFORMATION(#81)
SHAPE_REPRESENTATION_RELATIONSHIP()
);
#134=(
REPRESENTATION_RELATIONSHIP($,$,#9543,#9538)
REPRESENTATION_RELATIONSHIP_WITH_TRANSFORMATION(#82)
SHAPE_REPRESENTATION_RELATIONSHIP()
);
#135=(
REPRESENTATION_RELATIONSHIP($,$,#9549,#9538)
REPRESENTATION_RELATIONSHIP_WITH_TRANSFORMATION(#83)
SHAPE_REPRESENTATION_RELATIONSHIP()
);
#136=(
REPRESENTATION_RELATIONSHIP($,$,#9549,#9538)
REPRESENTATION_RELATIONSHIP_WITH_TRANSFORMATION(#84)
SHAPE_REPRESENTATION_RELATIONSHIP()
);
#137=(
REPRESENTATION_RELATIONSHIP($,$,#9549,#9538)
REPRESENTATION_RELATIONSHIP_WITH_TRANSFORMATION(#85)
SHAPE_REPRESENTATION_RELATIONSHIP()
);
#138=(
REPRESENTATION_RELATIONSHIP($,$,#9549,#9538)
REPRESENTATION_RELATIONSHIP_WITH_TRANSFORMATION(#86)
SHAPE_REPRESENTATION_RELATIONSHIP()
);
#139=(
REPRESENTATION_RELATIONSHIP($,$,#9549,#9538)
REPRESENTATION_RELATIONSHIP_WITH_TRANSFORMATION(#87)
SHAPE_REPRESENTATION_RELATIONSHIP()
);
#140=(
REPRESENTATION_RELATIONSHIP($,$,#9549,#9538)
REPRESENTATION_RELATIONSHIP_WITH_TRANSFORMATION(#88)
SHAPE_REPRESENTATION_RELATIONSHIP()
);
#141=(
REPRESENTATION_RELATIONSHIP($,$,#9549,#9538)
REPRESENTATION_RELATIONSHIP_WITH_TRANSFORMATION(#89)
SHAPE_REPRESENTATION_RELATIONSHIP()
);
#142=(
REPRESENTATION_RELATIONSHIP($,$,#9549,#9538)
REPRESENTATION_RELATIONSHIP_WITH_TRANSFORMATION(#90)
SHAPE_REPRESENTATION_RELATIONSHIP()
);
#143=(
REPRESENTATION_RELATIONSHIP($,$,#9551,#9550)
REPRESENTATION_RELATIONSHIP_WITH_TRANSFORMATION(#91)
SHAPE_REPRESENTATION_RELATIONSHIP()
);
#144=(
REPRESENTATION_RELATIONSHIP($,$,#9552,#9550)
REPRESENTATION_RELATIONSHIP_WITH_TRANSFORMATION(#92)
SHAPE_REPRESENTATION_RELATIONSHIP()
);
#145=(
REPRESENTATION_RELATIONSHIP($,$,#9553,#9550)
REPRESENTATION_RELATIONSHIP_WITH_TRANSFORMATION(#93)
SHAPE_REPRESENTATION_RELATIONSHIP()
);
#146=(
REPRESENTATION_RELATIONSHIP($,$,#9555,#9554)
REPRESENTATION_RELATIONSHIP_WITH_TRANSFORMATION(#94)
SHAPE_REPRESENTATION_RELATIONSHIP()
);
#147=(
REPRESENTATION_RELATIONSHIP($,$,#9521,#9520)
REPRESENTATION_RELATIONSHIP_WITH_TRANSFORMATION(#95)
SHAPE_REPRESENTATION_RELATIONSHIP()
);
#148=(
REPRESENTATION_RELATIONSHIP($,$,#9538,#9520)
REPRESENTATION_RELATIONSHIP_WITH_TRANSFORMATION(#96)
SHAPE_REPRESENTATION_RELATIONSHIP()
);
#149=(
REPRESENTATION_RELATIONSHIP($,$,#9550,#9520)
REPRESENTATION_RELATIONSHIP_WITH_TRANSFORMATION(#97)
SHAPE_REPRESENTATION_RELATIONSHIP()
);
#150=(
REPRESENTATION_RELATIONSHIP($,$,#9554,#9520)
REPRESENTATION_RELATIONSHIP_WITH_TRANSFORMATION(#98)
SHAPE_REPRESENTATION_RELATIONSHIP()
);
#151=CONTEXT_DEPENDENT_SHAPE_REPRESENTATION(#99,#9450);
#152=CONTEXT_DEPENDENT_SHAPE_REPRESENTATION(#100,#9451);
#153=CONTEXT_DEPENDENT_SHAPE_REPRESENTATION(#101,#9452);
#154=CONTEXT_DEPENDENT_SHAPE_REPRESENTATION(#102,#9453);
#155=CONTEXT_DEPENDENT_SHAPE_REPRESENTATION(#103,#9454);
#156=CONTEXT_DEPENDENT_SHAPE_REPRESENTATION(#104,#9455);
#157=CONTEXT_DEPENDENT_SHAPE_REPRESENTATION(#105,#9456);
#158=CONTEXT_DEPENDENT_SHAPE_REPRESENTATION(#106,#9457);
#159=CONTEXT_DEPENDENT_SHAPE_REPRESENTATION(#107,#9458);
#160=CONTEXT_DEPENDENT_SHAPE_REPRESENTATION(#108,#9459);
#161=CONTEXT_DEPENDENT_SHAPE_REPRESENTATION(#109,#9460);
#162=CONTEXT_DEPENDENT_SHAPE_REPRESENTATION(#110,#9461);
#163=CONTEXT_DEPENDENT_SHAPE_REPRESENTATION(#111,#9462);
#164=CONTEXT_DEPENDENT_SHAPE_REPRESENTATION(#112,#9463);
#165=CONTEXT_DEPENDENT_SHAPE_REPRESENTATION(#113,#9464);
#166=CONTEXT_DEPENDENT_SHAPE_REPRESENTATION(#114,#9465);
#167=CONTEXT_DEPENDENT_SHAPE_REPRESENTATION(#115,#9466);
#168=CONTEXT_DEPENDENT_SHAPE_REPRESENTATION(#116,#9467);
#169=CONTEXT_DEPENDENT_SHAPE_REPRESENTATION(#117,#9468);
#170=CONTEXT_DEPENDENT_SHAPE_REPRESENTATION(#118,#9469);
#171=CONTEXT_DEPENDENT_SHAPE_REPRESENTATION(#119,#9470);
#172=CONTEXT_DEPENDENT_SHAPE_REPRESENTATION(#120,#9471);
#173=CONTEXT_DEPENDENT_SHAPE_REPRESENTATION(#121,#9472);
#174=CONTEXT_DEPENDENT_SHAPE_REPRESENTATION(#122,#9473);
#175=CONTEXT_DEPENDENT_SHAPE_REPRESENTATION(#123,#9474);
#176=CONTEXT_DEPENDENT_SHAPE_REPRESENTATION(#124,#9486);
#177=CONTEXT_DEPENDENT_SHAPE_REPRESENTATION(#125,#9487);
#178=CONTEXT_DEPENDENT_SHAPE_REPRESENTATION(#126,#9488);
#179=CONTEXT_DEPENDENT_SHAPE_REPRESENTATION(#127,#9489);
#180=CONTEXT_DEPENDENT_SHAPE_REPRESENTATION(#128,#9490);
#181=CONTEXT_DEPENDENT_SHAPE_REPRESENTATION(#129,#9492);
#182=CONTEXT_DEPENDENT_SHAPE_REPRESENTATION(#130,#9493);
#183=CONTEXT_DEPENDENT_SHAPE_REPRESENTATION(#131,#9494);
#184=CONTEXT_DEPENDENT_SHAPE_REPRESENTATION(#132,#9495);
#185=CONTEXT_DEPENDENT_SHAPE_REPRESENTATION(#133,#9496);
#186=CONTEXT_DEPENDENT_SHAPE_REPRESENTATION(#134,#9497);
#187=CONTEXT_DEPENDENT_SHAPE_REPRESENTATION(#135,#9498);
#188=CONTEXT_DEPENDENT_SHAPE_REPRESENTATION(#136,#9499);
#189=CONTEXT_DEPENDENT_SHAPE_REPRESENTATION(#137,#9500);
#190=CONTEXT_DEPENDENT_SHAPE_REPRESENTATION(#138,#9501);
#191=CONTEXT_DEPENDENT_SHAPE_REPRESENTATION(#139,#9502);
#192=CONTEXT_DEPENDENT_SHAPE_REPRESENTATION(#140,#9503);
#193=CONTEXT_DEPENDENT_SHAPE_REPRESENTATION(#141,#9504);
#194=CONTEXT_DEPENDENT_SHAPE_REPRESENTATION(#142,#9505);
#195=CONTEXT_DEPENDENT_SHAPE_REPRESENTATION(#143,#9510);
#196=CONTEXT_DEPENDENT_SHAPE_REPRESENTATION(#144,#9511);
#197=CONTEXT_DEPENDENT_SHAPE_REPRESENTATION(#145,#9512);
#198=CONTEXT_DEPENDENT_SHAPE_REPRESENTATION(#146,#9515);
#199=CONTEXT_DEPENDENT_SHAPE_REPRESENTATION(#147,#9516);
#200=CONTEXT_DEPENDENT_SHAPE_REPRESENTATION(#148,#9517);
#201=CONTEXT_DEPENDENT_SHAPE_REPRESENTATION(#149,#9518);
#202=CONTEXT_DEPENDENT_SHAPE_REPRESENTATION(#150,#9519);
#203=NEXT_ASSEMBLY_USAGE_OCCURRENCE('Side plate:1','Side plate:1',
'Side plate:1',#9558,#9559,'Side plate:1');
#204=NEXT_ASSEMBLY_USAGE_OCCURRENCE('Side plate (1):1',
'Side plate (1):1','Side plate (1):1',#9558,#9560,'Side plate (1):1');
#205=NEXT_ASSEMBLY_USAGE_OCCURRENCE('Hook bridge:1','Hook bridge:1',
'Hook bridge:1',#9558,#9561,'Hook bridge:1');
#206=NEXT_ASSEMBLY_USAGE_OCCURRENCE('Eye axle sleeve:1',
'Eye axle sleeve:1','Eye axle sleeve:1',#9558,#9562,'Eye axle sleeve:1');
#207=NEXT_ASSEMBLY_USAGE_OCCURRENCE('Sheave axle:1','Sheave axle:1',
'Sheave axle:1',#9558,#9563,'Sheave axle:1');
#208=NEXT_ASSEMBLY_USAGE_OCCURRENCE('Axle keeper:1','Axle keeper:1',
'Axle keeper:1',#9558,#9564,'Axle keeper:1');
#209=NEXT_ASSEMBLY_USAGE_OCCURRENCE('Outer inner-race spacer:1',
'Outer inner-race spacer:1','Outer inner-race spacer:1',#9558,#9565,
'Outer inner-race spacer:1');
#210=NEXT_ASSEMBLY_USAGE_OCCURRENCE('Outer inner-race spacer (1):1',
'Outer inner-race spacer (1):1','Outer inner-race spacer (1):1',#9558,#9566,
'Outer inner-race spacer (1):1');
#211=NEXT_ASSEMBLY_USAGE_OCCURRENCE('Central inner-race spacer:1',
'Central inner-race spacer:1','Central inner-race spacer:1',#9558,#9567,
'Central inner-race spacer:1');
#212=NEXT_ASSEMBLY_USAGE_OCCURRENCE('Hook bushing:1','Hook bushing:1',
'Hook bushing:1',#9558,#9568,'Hook bushing:1');
#213=NEXT_ASSEMBLY_USAGE_OCCURRENCE('Eye spacer:1','Eye spacer:1',
'Eye spacer:1',#9558,#9569,'Eye spacer:1');
#214=NEXT_ASSEMBLY_USAGE_OCCURRENCE('Eye spacer (1):1',
'Eye spacer (1):1','Eye spacer (1):1',#9558,#9570,'Eye spacer (1):1');
#215=NEXT_ASSEMBLY_USAGE_OCCURRENCE('Flat Washer - M8:2',
'Flat Washer - M8:2','Flat Washer - M8:2',#9558,#9572,
'Flat Washer - M8:2');
#216=NEXT_ASSEMBLY_USAGE_OCCURRENCE('M8x75 cross bolt:2',
'M8x75 cross bolt:2','M8x75 cross bolt:2',#9558,#9571,
'M8x75 cross bolt:2');
#217=NEXT_ASSEMBLY_USAGE_OCCURRENCE('Flat Washer - M8:3',
'Flat Washer - M8:3','Flat Washer - M8:3',#9558,#9572,
'Flat Washer - M8:3');
#218=NEXT_ASSEMBLY_USAGE_OCCURRENCE('Hex Nut - M8:2','Hex Nut - M8:2',
'Hex Nut - M8:2',#9558,#9573,'Hex Nut - M8:2');
#219=NEXT_ASSEMBLY_USAGE_OCCURRENCE('Flat Washer - M8:4',
'Flat Washer - M8:4','Flat Washer - M8:4',#9558,#9572,
'Flat Washer - M8:4');
#220=NEXT_ASSEMBLY_USAGE_OCCURRENCE('M8x75 cross bolt:3',
'M8x75 cross bolt:3','M8x75 cross bolt:3',#9558,#9571,
'M8x75 cross bolt:3');
#221=NEXT_ASSEMBLY_USAGE_OCCURRENCE('Flat Washer - M8:5',
'Flat Washer - M8:5','Flat Washer - M8:5',#9558,#9572,
'Flat Washer - M8:5');
#222=NEXT_ASSEMBLY_USAGE_OCCURRENCE('Hex Nut - M8:3','Hex Nut - M8:3',
'Hex Nut - M8:3',#9558,#9573,'Hex Nut - M8:3');
#223=NEXT_ASSEMBLY_USAGE_OCCURRENCE('Flat Washer - M8:6',
'Flat Washer - M8:6','Flat Washer - M8:6',#9558,#9572,
'Flat Washer - M8:6');
#224=NEXT_ASSEMBLY_USAGE_OCCURRENCE('M8x75 cross bolt:4',
'M8x75 cross bolt:4','M8x75 cross bolt:4',#9558,#9571,
'M8x75 cross bolt:4');
#225=NEXT_ASSEMBLY_USAGE_OCCURRENCE('Flat Washer - M8:7',
'Flat Washer - M8:7','Flat Washer - M8:7',#9558,#9572,
'Flat Washer - M8:7');
#226=NEXT_ASSEMBLY_USAGE_OCCURRENCE('Hex Nut - M8:4','Hex Nut - M8:4',
'Hex Nut - M8:4',#9558,#9573,'Hex Nut - M8:4');
#227=NEXT_ASSEMBLY_USAGE_OCCURRENCE('Cap Screw - M8x30:2',
'Cap Screw - M8x30:2','Cap Screw - M8x30:2',#9558,#9574,
'Cap Screw - M8x30:2');
#228=NEXT_ASSEMBLY_USAGE_OCCURRENCE('Inner ring:1','Inner ring:1',
'Inner ring:1',#9580,#9581,'Inner ring:1');
#229=NEXT_ASSEMBLY_USAGE_OCCURRENCE('Outer ring:1','Outer ring:1',
'Outer ring:1',#9580,#9582,'Outer ring:1');
#230=NEXT_ASSEMBLY_USAGE_OCCURRENCE('Balls:1','Balls:1','Balls:1',#9580,
#9583,'Balls:1');
#231=NEXT_ASSEMBLY_USAGE_OCCURRENCE('Cage:1','Cage:1','Cage:1',#9580,#9584,
'Cage:1');
#232=NEXT_ASSEMBLY_USAGE_OCCURRENCE('Seals 2RS:1','Seals 2RS:1',
'Seals 2RS:1',#9580,#9585,'Seals 2RS:1');
#233=NEXT_ASSEMBLY_USAGE_OCCURRENCE('Sheave:1','Sheave:1','Sheave:1',#9575,
#9576,'Sheave:1');
#234=NEXT_ASSEMBLY_USAGE_OCCURRENCE('Outer race spacer:1',
'Outer race spacer:1','Outer race spacer:1',#9575,#9577,
'Outer race spacer:1');
#235=NEXT_ASSEMBLY_USAGE_OCCURRENCE('Sheave cap:1','Sheave cap:1',
'Sheave cap:1',#9575,#9578,'Sheave cap:1');
#236=NEXT_ASSEMBLY_USAGE_OCCURRENCE('Sheave cap (1):1',
'Sheave cap (1):1','Sheave cap (1):1',#9575,#9579,'Sheave cap (1):1');
#237=NEXT_ASSEMBLY_USAGE_OCCURRENCE(
'Sealed Ball Bearing - 20 x 47 x 14 mm:2',
'Sealed Ball Bearing - 20 x 47 x 14 mm:2',
'Sealed Ball Bearing - 20 x 47 x 14 mm:2',#9575,#9580,
'Sealed Ball Bearing - 20 x 47 x 14 mm:2');
#238=NEXT_ASSEMBLY_USAGE_OCCURRENCE(
'Sealed Ball Bearing - 20 x 47 x 14 mm:3',
'Sealed Ball Bearing - 20 x 47 x 14 mm:3',
'Sealed Ball Bearing - 20 x 47 x 14 mm:3',#9575,#9580,
'Sealed Ball Bearing - 20 x 47 x 14 mm:3');
#239=NEXT_ASSEMBLY_USAGE_OCCURRENCE('M4x10 Cap Screw:2',
'M4x10 Cap Screw:2','M4x10 Cap Screw:2',#9575,#9586,'M4x10 Cap Screw:2');
#240=NEXT_ASSEMBLY_USAGE_OCCURRENCE('M4x10 Cap Screw:3',
'M4x10 Cap Screw:3','M4x10 Cap Screw:3',#9575,#9586,'M4x10 Cap Screw:3');
#241=NEXT_ASSEMBLY_USAGE_OCCURRENCE('M4x10 Cap Screw:4',
'M4x10 Cap Screw:4','M4x10 Cap Screw:4',#9575,#9586,'M4x10 Cap Screw:4');
#242=NEXT_ASSEMBLY_USAGE_OCCURRENCE('M4x10 Cap Screw:5',
'M4x10 Cap Screw:5','M4x10 Cap Screw:5',#9575,#9586,'M4x10 Cap Screw:5');
#243=NEXT_ASSEMBLY_USAGE_OCCURRENCE('M4x10 Cap Screw:6',
'M4x10 Cap Screw:6','M4x10 Cap Screw:6',#9575,#9586,'M4x10 Cap Screw:6');
#244=NEXT_ASSEMBLY_USAGE_OCCURRENCE('M4x10 Cap Screw:7',
'M4x10 Cap Screw:7','M4x10 Cap Screw:7',#9575,#9586,'M4x10 Cap Screw:7');
#245=NEXT_ASSEMBLY_USAGE_OCCURRENCE('M4x10 Cap Screw:8',
'M4x10 Cap Screw:8','M4x10 Cap Screw:8',#9575,#9586,'M4x10 Cap Screw:8');
#246=NEXT_ASSEMBLY_USAGE_OCCURRENCE('M4x10 Cap Screw:9',
'M4x10 Cap Screw:9','M4x10 Cap Screw:9',#9575,#9586,'M4x10 Cap Screw:9');
#247=NEXT_ASSEMBLY_USAGE_OCCURRENCE('Hook:1','Hook:1','Hook:1',#9587,#9588,
'Hook:1');
#248=NEXT_ASSEMBLY_USAGE_OCCURRENCE('Swivel thrust washer:1',
'Swivel thrust washer:1','Swivel thrust washer:1',#9587,#9589,
'Swivel thrust washer:1');
#249=NEXT_ASSEMBLY_USAGE_OCCURRENCE('M16 hook retaining nut:1',
'M16 hook retaining nut:1','M16 hook retaining nut:1',#9587,#9590,
'M16 hook retaining nut:1');
#250=NEXT_ASSEMBLY_USAGE_OCCURRENCE('Lifting eye link:1',
'Lifting eye link:1','Lifting eye link:1',#9591,#9592,
'Lifting eye link:1');
#251=NEXT_ASSEMBLY_USAGE_OCCURRENCE('Side plates and axles:1',
'Side plates and axles:1','Side plates and axles:1',#9557,#9558,
'Side plates and axles:1');
#252=NEXT_ASSEMBLY_USAGE_OCCURRENCE('Rope sheave:1','Rope sheave:1',
'Rope sheave:1',#9557,#9575,'Rope sheave:1');
#253=NEXT_ASSEMBLY_USAGE_OCCURRENCE('Swivel hook:1','Swivel hook:1',
'Swivel hook:1',#9557,#9587,'Swivel hook:1');
#254=NEXT_ASSEMBLY_USAGE_OCCURRENCE('Lifting eye:1','Lifting eye:1',
'Lifting eye:1',#9557,#9591,'Lifting eye:1');
#255=(
BOUNDED_CURVE()
B_SPLINE_CURVE(2,(#8141,#8142,#8143),.UNSPECIFIED.,.F.,.F.)
B_SPLINE_CURVE_WITH_KNOTS((3,3),(0.14973948338295,0.97160236658079),
 .UNSPECIFIED.)
CURVE()
GEOMETRIC_REPRESENTATION_ITEM()
RATIONAL_B_SPLINE_CURVE((1.07140024848292,1.23714644374248,1.07140024848292))
REPRESENTATION_ITEM('')
);
#256=(
BOUNDED_CURVE()
B_SPLINE_CURVE(2,(#8145,#8146,#8147),.UNSPECIFIED.,.F.,.F.)
B_SPLINE_CURVE_WITH_KNOTS((3,3),(0.14973948338295,0.971602366580789),
 .UNSPECIFIED.)
CURVE()
GEOMETRIC_REPRESENTATION_ITEM()
RATIONAL_B_SPLINE_CURVE((1.07140024848292,1.23714644374248,1.07140024848292))
REPRESENTATION_ITEM('')
);
#257=(
BOUNDED_CURVE()
B_SPLINE_CURVE(2,(#8152,#8153,#8154),.UNSPECIFIED.,.F.,.F.)
B_SPLINE_CURVE_WITH_KNOTS((3,3),(0.14973948338295,0.97160236658079),
 .UNSPECIFIED.)
CURVE()
GEOMETRIC_REPRESENTATION_ITEM()
RATIONAL_B_SPLINE_CURVE((1.07140024848292,1.23714644374248,1.07140024848292))
REPRESENTATION_ITEM('')
);
#258=(
BOUNDED_CURVE()
B_SPLINE_CURVE(2,(#8156,#8157,#8158),.UNSPECIFIED.,.F.,.F.)
B_SPLINE_CURVE_WITH_KNOTS((3,3),(0.14973948338295,0.97160236658079),
 .UNSPECIFIED.)
CURVE()
GEOMETRIC_REPRESENTATION_ITEM()
RATIONAL_B_SPLINE_CURVE((1.07140024848292,1.23714644374248,1.07140024848292))
REPRESENTATION_ITEM('')
);
#259=(
BOUNDED_CURVE()
B_SPLINE_CURVE(2,(#8160,#8161,#8162),.UNSPECIFIED.,.F.,.F.)
B_SPLINE_CURVE_WITH_KNOTS((3,3),(0.14973948338295,0.971602366580789),
 .UNSPECIFIED.)
CURVE()
GEOMETRIC_REPRESENTATION_ITEM()
RATIONAL_B_SPLINE_CURVE((1.07140024848292,1.23714644374248,1.07140024848292))
REPRESENTATION_ITEM('')
);
#260=(
BOUNDED_CURVE()
B_SPLINE_CURVE(2,(#8163,#8164,#8165),.UNSPECIFIED.,.F.,.F.)
B_SPLINE_CURVE_WITH_KNOTS((3,3),(0.14973948338295,0.97160236658079),
 .UNSPECIFIED.)
CURVE()
GEOMETRIC_REPRESENTATION_ITEM()
RATIONAL_B_SPLINE_CURVE((1.07140024848292,1.23714644374248,1.07140024848292))
REPRESENTATION_ITEM('')
);
#261=(
BOUNDED_CURVE()
B_SPLINE_CURVE(2,(#8172,#8173,#8174),.UNSPECIFIED.,.F.,.F.)
B_SPLINE_CURVE_WITH_KNOTS((3,3),(0.14973948338295,0.97160236658079),
 .UNSPECIFIED.)
CURVE()
GEOMETRIC_REPRESENTATION_ITEM()
RATIONAL_B_SPLINE_CURVE((1.07140024848292,1.23714644374248,1.07140024848292))
REPRESENTATION_ITEM('')
);
#262=(
BOUNDED_CURVE()
B_SPLINE_CURVE(2,(#8176,#8177,#8178),.UNSPECIFIED.,.F.,.F.)
B_SPLINE_CURVE_WITH_KNOTS((3,3),(0.14973948338295,0.97160236658079),
 .UNSPECIFIED.)
CURVE()
GEOMETRIC_REPRESENTATION_ITEM()
RATIONAL_B_SPLINE_CURVE((1.07140024848292,1.23714644374248,1.07140024848292))
REPRESENTATION_ITEM('')
);
#263=(
BOUNDED_CURVE()
B_SPLINE_CURVE(2,(#8180,#8181,#8182),.UNSPECIFIED.,.F.,.F.)
B_SPLINE_CURVE_WITH_KNOTS((3,3),(0.14973948338295,0.971602366580789),
 .UNSPECIFIED.)
CURVE()
GEOMETRIC_REPRESENTATION_ITEM()
RATIONAL_B_SPLINE_CURVE((1.07140024848292,1.23714644374248,1.07140024848292))
REPRESENTATION_ITEM('')
);
#264=(
BOUNDED_CURVE()
B_SPLINE_CURVE(2,(#8184,#8185,#8186),.UNSPECIFIED.,.F.,.F.)
B_SPLINE_CURVE_WITH_KNOTS((3,3),(0.14973948338295,0.97160236658079),
 .UNSPECIFIED.)
CURVE()
GEOMETRIC_REPRESENTATION_ITEM()
RATIONAL_B_SPLINE_CURVE((1.07140024848292,1.23714644374248,1.07140024848292))
REPRESENTATION_ITEM('')
);
#265=(
BOUNDED_CURVE()
B_SPLINE_CURVE(2,(#8188,#8189,#8190),.UNSPECIFIED.,.F.,.F.)
B_SPLINE_CURVE_WITH_KNOTS((3,3),(0.14973948338295,0.97160236658079),
 .UNSPECIFIED.)
CURVE()
GEOMETRIC_REPRESENTATION_ITEM()
RATIONAL_B_SPLINE_CURVE((1.07140024848292,1.23714644374248,1.07140024848292))
REPRESENTATION_ITEM('')
);
#266=(
BOUNDED_CURVE()
B_SPLINE_CURVE(2,(#8191,#8192,#8193),.UNSPECIFIED.,.F.,.F.)
B_SPLINE_CURVE_WITH_KNOTS((3,3),(0.14973948338295,0.971602366580789),
 .UNSPECIFIED.)
CURVE()
GEOMETRIC_REPRESENTATION_ITEM()
RATIONAL_B_SPLINE_CURVE((1.07140024848292,1.23714644374248,1.07140024848292))
REPRESENTATION_ITEM('')
);
#267=CONICAL_SURFACE('',#5500,0.625,0.785398163397448);
#268=CONICAL_SURFACE('',#5504,0.635,0.785398163397449);
#269=CONICAL_SURFACE('',#5508,0.41,0.463647609000806);
#270=CONICAL_SURFACE('',#5521,0.734027674973257,1.0471975511966);
#271=CONICAL_SURFACE('',#5523,0.734027674973257,1.0471975511966);
#272=CONICAL_SURFACE('',#5539,0.625,0.785398163397448);
#273=CONICAL_SURFACE('',#5543,0.635,0.785398163397449);
#274=CONICAL_SURFACE('',#5547,0.41,0.463647609000806);
#275=CONICAL_SURFACE('',#5551,0.36,0.785398163397448);
#276=CONICAL_SURFACE('',#5601,4.7,0.785398163397448);
#277=CONICAL_SURFACE('',#5604,4.7,0.785398163397448);
#278=CONICAL_SURFACE('',#5695,1.05,0.785398163397449);
#279=CONICAL_SURFACE('',#5702,1.05,0.785398163397449);
#280=CONICAL_SURFACE('',#5715,2.3,0.785398163397449);
#281=CONICAL_SURFACE('',#5719,2.3,0.785398163397449);
#282=CONICAL_SURFACE('',#5829,0.325,0.785398163397448);
#283=CONICAL_SURFACE('',#5833,0.335,0.785398163397448);
#284=CONICAL_SURFACE('',#5837,0.21,0.463647609000806);
#285=ORIENTED_CLOSED_SHELL('',*,#4899,.F.);
#286=ORIENTED_CLOSED_SHELL('',*,#4904,.F.);
#287=ORIENTED_CLOSED_SHELL('',*,#4922,.F.);
#288=BREP_WITH_VOIDS('Body1',#4900,(#285));
#289=BREP_WITH_VOIDS('Body1',#4903,(#286));
#290=BREP_WITH_VOIDS('Body1',#4923,(#287));
#291=SHAPE_REPRESENTATION_RELATIONSHIP('SRR','None',#9522,#321);
#292=SHAPE_REPRESENTATION_RELATIONSHIP('SRR','None',#9523,#322);
#293=SHAPE_REPRESENTATION_RELATIONSHIP('SRR','None',#9524,#323);
#294=SHAPE_REPRESENTATION_RELATIONSHIP('SRR','None',#9525,#324);
#295=SHAPE_REPRESENTATION_RELATIONSHIP('SRR','None',#9526,#325);
#296=SHAPE_REPRESENTATION_RELATIONSHIP('SRR','None',#9527,#326);
#297=SHAPE_REPRESENTATION_RELATIONSHIP('SRR','None',#9528,#327);
#298=SHAPE_REPRESENTATION_RELATIONSHIP('SRR','None',#9529,#328);
#299=SHAPE_REPRESENTATION_RELATIONSHIP('SRR','None',#9530,#329);
#300=SHAPE_REPRESENTATION_RELATIONSHIP('SRR','None',#9531,#330);
#301=SHAPE_REPRESENTATION_RELATIONSHIP('SRR','None',#9532,#331);
#302=SHAPE_REPRESENTATION_RELATIONSHIP('SRR','None',#9533,#332);
#303=SHAPE_REPRESENTATION_RELATIONSHIP('SRR','None',#9534,#333);
#304=SHAPE_REPRESENTATION_RELATIONSHIP('SRR','None',#9535,#334);
#305=SHAPE_REPRESENTATION_RELATIONSHIP('SRR','None',#9536,#335);
#306=SHAPE_REPRESENTATION_RELATIONSHIP('SRR','None',#9537,#336);
#307=SHAPE_REPRESENTATION_RELATIONSHIP('SRR','None',#9539,#337);
#308=SHAPE_REPRESENTATION_RELATIONSHIP('SRR','None',#9540,#338);
#309=SHAPE_REPRESENTATION_RELATIONSHIP('SRR','None',#9541,#339);
#310=SHAPE_REPRESENTATION_RELATIONSHIP('SRR','None',#9542,#340);
#311=SHAPE_REPRESENTATION_RELATIONSHIP('SRR','None',#9544,#341);
#312=SHAPE_REPRESENTATION_RELATIONSHIP('SRR','None',#9545,#342);
#313=SHAPE_REPRESENTATION_RELATIONSHIP('SRR','None',#9546,#343);
#314=SHAPE_REPRESENTATION_RELATIONSHIP('SRR','None',#9547,#344);
#315=SHAPE_REPRESENTATION_RELATIONSHIP('SRR','None',#9548,#345);
#316=SHAPE_REPRESENTATION_RELATIONSHIP('SRR','None',#9549,#346);
#317=SHAPE_REPRESENTATION_RELATIONSHIP('SRR','None',#9551,#347);
#318=SHAPE_REPRESENTATION_RELATIONSHIP('SRR','None',#9552,#348);
#319=SHAPE_REPRESENTATION_RELATIONSHIP('SRR','None',#9553,#349);
#320=SHAPE_REPRESENTATION_RELATIONSHIP('SRR','None',#9555,#350);
#321=ADVANCED_BREP_SHAPE_REPRESENTATION('',(#389),#9357);
#322=ADVANCED_BREP_SHAPE_REPRESENTATION('',(#390),#9358);
#323=ADVANCED_BREP_SHAPE_REPRESENTATION('',(#391),#9359);
#324=ADVANCED_BREP_SHAPE_REPRESENTATION('',(#392),#9360);
#325=ADVANCED_BREP_SHAPE_REPRESENTATION('',(#393),#9361);
#326=ADVANCED_BREP_SHAPE_REPRESENTATION('',(#394),#9362);
#327=ADVANCED_BREP_SHAPE_REPRESENTATION('',(#395),#9363);
#328=ADVANCED_BREP_SHAPE_REPRESENTATION('',(#396),#9364);
#329=ADVANCED_BREP_SHAPE_REPRESENTATION('',(#397),#9365);
#330=ADVANCED_BREP_SHAPE_REPRESENTATION('',(#398),#9366);
#331=ADVANCED_BREP_SHAPE_REPRESENTATION('',(#399),#9367);
#332=ADVANCED_BREP_SHAPE_REPRESENTATION('',(#400),#9368);
#333=ADVANCED_BREP_SHAPE_REPRESENTATION('',(#288),#9369);
#334=ADVANCED_BREP_SHAPE_REPRESENTATION('',(#401),#9370);
#335=ADVANCED_BREP_SHAPE_REPRESENTATION('',(#402),#9371);
#336=ADVANCED_BREP_SHAPE_REPRESENTATION('',(#289),#9372);
#337=ADVANCED_BREP_SHAPE_REPRESENTATION('',(#403),#9374);
#338=ADVANCED_BREP_SHAPE_REPRESENTATION('',(#404),#9375);
#339=ADVANCED_BREP_SHAPE_REPRESENTATION('',(#405),#9376);
#340=ADVANCED_BREP_SHAPE_REPRESENTATION('',(#406),#9377);
#341=ADVANCED_BREP_SHAPE_REPRESENTATION('',(#407),#9379);
#342=ADVANCED_BREP_SHAPE_REPRESENTATION('',(#408),#9380);
#343=ADVANCED_BREP_SHAPE_REPRESENTATION('',(#409,#410,#411,#412,#413,#414,
#415,#416),#9381);
#344=ADVANCED_BREP_SHAPE_REPRESENTATION('',(#417),#9382);
#345=ADVANCED_BREP_SHAPE_REPRESENTATION('',(#418,#419),#9383);
#346=ADVANCED_BREP_SHAPE_REPRESENTATION('',(#290),#9384);
#347=ADVANCED_BREP_SHAPE_REPRESENTATION('',(#420),#9386);
#348=ADVANCED_BREP_SHAPE_REPRESENTATION('',(#421),#9387);
#349=ADVANCED_BREP_SHAPE_REPRESENTATION('',(#422),#9388);
#350=ADVANCED_BREP_SHAPE_REPRESENTATION('',(#423),#9390);
#351=STYLED_ITEM('',(#9752),#389);
#352=STYLED_ITEM('',(#9752),#390);
#353=STYLED_ITEM('',(#9773),#391);
#354=STYLED_ITEM('',(#9759),#392);
#355=STYLED_ITEM('',(#9759),#393);
#356=STYLED_ITEM('',(#9759),#394);
#357=STYLED_ITEM('',(#9745),#395);
#358=STYLED_ITEM('',(#9745),#396);
#359=STYLED_ITEM('',(#9745),#397);
#360=STYLED_ITEM('',(#9745),#398);
#361=STYLED_ITEM('',(#9745),#399);
#362=STYLED_ITEM('',(#9745),#400);
#363=STYLED_ITEM('',(#9766),#288);
#364=STYLED_ITEM('',(#9766),#401);
#365=STYLED_ITEM('',(#9766),#402);
#366=STYLED_ITEM('',(#9766),#289);
#367=STYLED_ITEM('',(#9752),#403);
#368=STYLED_ITEM('',(#9759),#404);
#369=STYLED_ITEM('',(#9773),#405);
#370=STYLED_ITEM('',(#9773),#406);
#371=STYLED_ITEM('',(#9759),#407);
#372=STYLED_ITEM('',(#9759),#408);
#373=STYLED_ITEM('',(#9759),#409);
#374=STYLED_ITEM('',(#9759),#410);
#375=STYLED_ITEM('',(#9759),#411);
#376=STYLED_ITEM('',(#9759),#412);
#377=STYLED_ITEM('',(#9759),#413);
#378=STYLED_ITEM('',(#9759),#414);
#379=STYLED_ITEM('',(#9759),#415);
#380=STYLED_ITEM('',(#9759),#416);
#381=STYLED_ITEM('',(#9759),#417);
#382=STYLED_ITEM('',(#9759),#418);
#383=STYLED_ITEM('',(#9759),#419);
#384=STYLED_ITEM('',(#9766),#290);
#385=STYLED_ITEM('',(#9745),#420);
#386=STYLED_ITEM('',(#9766),#421);
#387=STYLED_ITEM('',(#9766),#422);
#388=STYLED_ITEM('',(#9752),#423);
#389=MANIFOLD_SOLID_BREP('Body1',#4887);
#390=MANIFOLD_SOLID_BREP('Body1',#4888);
#391=MANIFOLD_SOLID_BREP('Body1',#4889);
#392=MANIFOLD_SOLID_BREP('Body1',#4890);
#393=MANIFOLD_SOLID_BREP('Body1',#4891);
#394=MANIFOLD_SOLID_BREP('Body1',#4892);
#395=MANIFOLD_SOLID_BREP('Body1',#4893);
#396=MANIFOLD_SOLID_BREP('Body1',#4894);
#397=MANIFOLD_SOLID_BREP('Body1',#4895);
#398=MANIFOLD_SOLID_BREP('Body1',#4896);
#399=MANIFOLD_SOLID_BREP('Body1',#4897);
#400=MANIFOLD_SOLID_BREP('Body1',#4898);
#401=MANIFOLD_SOLID_BREP('Body1',#4901);
#402=MANIFOLD_SOLID_BREP('Body1',#4902);
#403=MANIFOLD_SOLID_BREP('Body1',#4905);
#404=MANIFOLD_SOLID_BREP('Body1',#4906);
#405=MANIFOLD_SOLID_BREP('Body1',#4907);
#406=MANIFOLD_SOLID_BREP('Body1',#4908);
#407=MANIFOLD_SOLID_BREP('Body1',#4909);
#408=MANIFOLD_SOLID_BREP('Body1',#4910);
#409=MANIFOLD_SOLID_BREP('Body1',#4911);
#410=MANIFOLD_SOLID_BREP('Body2',#4912);
#411=MANIFOLD_SOLID_BREP('Body3',#4913);
#412=MANIFOLD_SOLID_BREP('Body4',#4914);
#413=MANIFOLD_SOLID_BREP('Body5',#4915);
#414=MANIFOLD_SOLID_BREP('Body6',#4916);
#415=MANIFOLD_SOLID_BREP('Body7',#4917);
#416=MANIFOLD_SOLID_BREP('Body8',#4918);
#417=MANIFOLD_SOLID_BREP('Continuous crown cage',#4919);
#418=MANIFOLD_SOLID_BREP('Body1',#4920);
#419=MANIFOLD_SOLID_BREP('Body2',#4921);
#420=MANIFOLD_SOLID_BREP('Body1',#4924);
#421=MANIFOLD_SOLID_BREP('Body1',#4925);
#422=MANIFOLD_SOLID_BREP('Body1',#4926);
#423=MANIFOLD_SOLID_BREP('Body1',#4927);
#424=LINE('',#7581,#712);
#425=LINE('',#7583,#713);
#426=LINE('',#7587,#714);
#427=LINE('',#7590,#715);
#428=LINE('',#7593,#716);
#429=LINE('',#7595,#717);
#430=LINE('',#7599,#718);
#431=LINE('',#7603,#719);
#432=LINE('',#7606,#720);
#433=LINE('',#7611,#721);
#434=LINE('',#7618,#722);
#435=LINE('',#7625,#723);
#436=LINE('',#7635,#724);
#437=LINE('',#7642,#725);
#438=LINE('',#7648,#726);
#439=LINE('',#7654,#727);
#440=LINE('',#7659,#728);
#441=LINE('',#7663,#729);
#442=LINE('',#7665,#730);
#443=LINE('',#7667,#731);
#444=LINE('',#7668,#732);
#445=LINE('',#7671,#733);
#446=LINE('',#7673,#734);
#447=LINE('',#7674,#735);
#448=LINE('',#7677,#736);
#449=LINE('',#7679,#737);
#450=LINE('',#7680,#738);
#451=LINE('',#7683,#739);
#452=LINE('',#7685,#740);
#453=LINE('',#7686,#741);
#454=LINE('',#7689,#742);
#455=LINE('',#7691,#743);
#456=LINE('',#7692,#744);
#457=LINE('',#7695,#745);
#458=LINE('',#7697,#746);
#459=LINE('',#7698,#747);
#460=LINE('',#7701,#748);
#461=LINE('',#7703,#749);
#462=LINE('',#7704,#750);
#463=LINE('',#7706,#751);
#464=LINE('',#7707,#752);
#465=LINE('',#7732,#753);
#466=LINE('',#7734,#754);
#467=LINE('',#7738,#755);
#468=LINE('',#7740,#756);
#469=LINE('',#7744,#757);
#470=LINE('',#7747,#758);
#471=LINE('',#7751,#759);
#472=LINE('',#7754,#760);
#473=LINE('',#7757,#761);
#474=LINE('',#7762,#762);
#475=LINE('',#7769,#763);
#476=LINE('',#7779,#764);
#477=LINE('',#7786,#765);
#478=LINE('',#7793,#766);
#479=LINE('',#7799,#767);
#480=LINE('',#7805,#768);
#481=LINE('',#7809,#769);
#482=LINE('',#7814,#770);
#483=LINE('',#7816,#771);
#484=LINE('',#7818,#772);
#485=LINE('',#7819,#773);
#486=LINE('',#7822,#774);
#487=LINE('',#7824,#775);
#488=LINE('',#7825,#776);
#489=LINE('',#7828,#777);
#490=LINE('',#7830,#778);
#491=LINE('',#7831,#779);
#492=LINE('',#7834,#780);
#493=LINE('',#7836,#781);
#494=LINE('',#7837,#782);
#495=LINE('',#7840,#783);
#496=LINE('',#7842,#784);
#497=LINE('',#7843,#785);
#498=LINE('',#7846,#786);
#499=LINE('',#7848,#787);
#500=LINE('',#7849,#788);
#501=LINE('',#7852,#789);
#502=LINE('',#7854,#790);
#503=LINE('',#7855,#791);
#504=LINE('',#7857,#792);
#505=LINE('',#7858,#793);
#506=LINE('',#7866,#794);
#507=LINE('',#7872,#795);
#508=LINE('',#7878,#796);
#509=LINE('',#7883,#797);
#510=LINE('',#7885,#798);
#511=LINE('',#7887,#799);
#512=LINE('',#7888,#800);
#513=LINE('',#7891,#801);
#514=LINE('',#7893,#802);
#515=LINE('',#7894,#803);
#516=LINE('',#7897,#804);
#517=LINE('',#7899,#805);
#518=LINE('',#7900,#806);
#519=LINE('',#7902,#807);
#520=LINE('',#7903,#808);
#521=LINE('',#7911,#809);
#522=LINE('',#7917,#810);
#523=LINE('',#7926,#811);
#524=LINE('',#7936,#812);
#525=LINE('',#7942,#813);
#526=LINE('',#7949,#814);
#527=LINE('',#7955,#815);
#528=LINE('',#7964,#816);
#529=LINE('',#7970,#817);
#530=LINE('',#7979,#818);
#531=LINE('',#7985,#819);
#532=LINE('',#7994,#820);
#533=LINE('',#8000,#821);
#534=LINE('',#8009,#822);
#535=LINE('',#8015,#823);
#536=LINE('',#8024,#824);
#537=LINE('',#8030,#825);
#538=LINE('',#8039,#826);
#539=LINE('',#8045,#827);
#540=LINE('',#8053,#828);
#541=LINE('',#8055,#829);
#542=LINE('',#8057,#830);
#543=LINE('',#8058,#831);
#544=LINE('',#8061,#832);
#545=LINE('',#8063,#833);
#546=LINE('',#8064,#834);
#547=LINE('',#8067,#835);
#548=LINE('',#8069,#836);
#549=LINE('',#8070,#837);
#550=LINE('',#8073,#838);
#551=LINE('',#8075,#839);
#552=LINE('',#8076,#840);
#553=LINE('',#8079,#841);
#554=LINE('',#8081,#842);
#555=LINE('',#8082,#843);
#556=LINE('',#8084,#844);
#557=LINE('',#8085,#845);
#558=LINE('',#8095,#846);
#559=LINE('',#8104,#847);
#560=LINE('',#8108,#848);
#561=LINE('',#8112,#849);
#562=LINE('',#8119,#850);
#563=LINE('',#8121,#851);
#564=LINE('',#8127,#852);
#565=LINE('',#8133,#853);
#566=LINE('',#8149,#854);
#567=LINE('',#8170,#855);
#568=LINE('',#8195,#856);
#569=LINE('',#8196,#857);
#570=LINE('',#8198,#858);
#571=LINE('',#8200,#859);
#572=LINE('',#8205,#860);
#573=LINE('',#8208,#861);
#574=LINE('',#8210,#862);
#575=LINE('',#8221,#863);
#576=LINE('',#8225,#864);
#577=LINE('',#8229,#865);
#578=LINE('',#8236,#866);
#579=LINE('',#8240,#867);
#580=LINE('',#8244,#868);
#581=LINE('',#8249,#869);
#582=LINE('',#8251,#870);
#583=LINE('',#8253,#871);
#584=LINE('',#8254,#872);
#585=LINE('',#8257,#873);
#586=LINE('',#8259,#874);
#587=LINE('',#8260,#875);
#588=LINE('',#8263,#876);
#589=LINE('',#8265,#877);
#590=LINE('',#8266,#878);
#591=LINE('',#8269,#879);
#592=LINE('',#8271,#880);
#593=LINE('',#8272,#881);
#594=LINE('',#8275,#882);
#595=LINE('',#8277,#883);
#596=LINE('',#8278,#884);
#597=LINE('',#8280,#885);
#598=LINE('',#8281,#886);
#599=LINE('',#8315,#887);
#600=LINE('',#8321,#888);
#601=LINE('',#8327,#889);
#602=LINE('',#8333,#890);
#603=LINE('',#8339,#891);
#604=LINE('',#8344,#892);
#605=LINE('',#8348,#893);
#606=LINE('',#8358,#894);
#607=LINE('',#8361,#895);
#608=LINE('',#8367,#896);
#609=LINE('',#8372,#897);
#610=LINE('',#8380,#898);
#611=LINE('',#8386,#899);
#612=LINE('',#8395,#900);
#613=LINE('',#8401,#901);
#614=LINE('',#8407,#902);
#615=LINE('',#8413,#903);
#616=LINE('',#8419,#904);
#617=LINE('',#8426,#905);
#618=LINE('',#8432,#906);
#619=LINE('',#8441,#907);
#620=LINE('',#8447,#908);
#621=LINE('',#8453,#909);
#622=LINE('',#8459,#910);
#623=LINE('',#8465,#911);
#624=LINE('',#8473,#912);
#625=LINE('',#8478,#913);
#626=LINE('',#8496,#914);
#627=LINE('',#8502,#915);
#628=LINE('',#8506,#916);
#629=LINE('',#8512,#917);
#630=LINE('',#8517,#918);
#631=LINE('',#8532,#919);
#632=LINE('',#8541,#920);
#633=LINE('',#8545,#921);
#634=LINE('',#8549,#922);
#635=LINE('',#8552,#923);
#636=LINE('',#8705,#924);
#637=LINE('',#9001,#925);
#638=LINE('',#9043,#926);
#639=LINE('',#9048,#927);
#640=LINE('',#9057,#928);
#641=LINE('',#9062,#929);
#642=LINE('',#9072,#930);
#643=LINE('',#9074,#931);
#644=LINE('',#9076,#932);
#645=LINE('',#9077,#933);
#646=LINE('',#9080,#934);
#647=LINE('',#9082,#935);
#648=LINE('',#9083,#936);
#649=LINE('',#9086,#937);
#650=LINE('',#9088,#938);
#651=LINE('',#9089,#939);
#652=LINE('',#9092,#940);
#653=LINE('',#9094,#941);
#654=LINE('',#9095,#942);
#655=LINE('',#9098,#943);
#656=LINE('',#9100,#944);
#657=LINE('',#9101,#945);
#658=LINE('',#9103,#946);
#659=LINE('',#9104,#947);
#660=LINE('',#9116,#948);
#661=LINE('',#9120,#949);
#662=LINE('',#9124,#950);
#663=LINE('',#9131,#951);
#664=LINE('',#9133,#952);
#665=LINE('',#9161,#953);
#666=LINE('',#9164,#954);
#667=LINE('',#9173,#955);
#668=LINE('',#9177,#956);
#669=LINE('',#9179,#957);
#670=LINE('',#9180,#958);
#671=LINE('',#9183,#959);
#672=LINE('',#9185,#960);
#673=LINE('',#9186,#961);
#674=LINE('',#9190,#962);
#675=LINE('',#9191,#963);
#676=LINE('',#9192,#964);
#677=LINE('',#9196,#965);
#678=LINE('',#9198,#966);
#679=LINE('',#9200,#967);
#680=LINE('',#9201,#968);
#681=LINE('',#9203,#969);
#682=LINE('',#9207,#970);
#683=LINE('',#9212,#971);
#684=LINE('',#9214,#972);
#685=LINE('',#9217,#973);
#686=LINE('',#9220,#974);
#687=LINE('',#9227,#975);
#688=LINE('',#9233,#976);
#689=LINE('',#9242,#977);
#690=LINE('',#9247,#978);
#691=LINE('',#9249,#979);
#692=LINE('',#9251,#980);
#693=LINE('',#9252,#981);
#694=LINE('',#9255,#982);
#695=LINE('',#9257,#983);
#696=LINE('',#9258,#984);
#697=LINE('',#9261,#985);
#698=LINE('',#9263,#986);
#699=LINE('',#9264,#987);
#700=LINE('',#9267,#988);
#701=LINE('',#9269,#989);
#702=LINE('',#9270,#990);
#703=LINE('',#9273,#991);
#704=LINE('',#9275,#992);
#705=LINE('',#9276,#993);
#706=LINE('',#9278,#994);
#707=LINE('',#9279,#995);
#708=LINE('',#9291,#996);
#709=LINE('',#9297,#997);
#710=LINE('',#9302,#998);
#711=LINE('',#9306,#999);
#712=VECTOR('',#5957,1.);
#713=VECTOR('',#5958,1.);
#714=VECTOR('',#5963,1.);
#715=VECTOR('',#5966,1.);
#716=VECTOR('',#5969,1.);
#717=VECTOR('',#5970,1.);
#718=VECTOR('',#5975,1.2);
#719=VECTOR('',#5980,1.);
#720=VECTOR('',#5983,1.);
#721=VECTOR('',#5988,0.9);
#722=VECTOR('',#5997,0.9);
#723=VECTOR('',#6006,0.9);
#724=VECTOR('',#6019,0.9);
#725=VECTOR('',#6028,0.425);
#726=VECTOR('',#6035,0.425);
#727=VECTOR('',#6042,0.425);
#728=VECTOR('',#6049,1.);
#729=VECTOR('',#6052,1.);
#730=VECTOR('',#6053,1.);
#731=VECTOR('',#6054,1.);
#732=VECTOR('',#6055,1.);
#733=VECTOR('',#6058,1.);
#734=VECTOR('',#6059,1.);
#735=VECTOR('',#6060,1.);
#736=VECTOR('',#6063,1.);
#737=VECTOR('',#6064,1.);
#738=VECTOR('',#6065,1.);
#739=VECTOR('',#6068,1.);
#740=VECTOR('',#6069,1.);
#741=VECTOR('',#6070,1.);
#742=VECTOR('',#6073,1.);
#743=VECTOR('',#6074,1.);
#744=VECTOR('',#6075,1.);
#745=VECTOR('',#6078,1.);
#746=VECTOR('',#6079,1.);
#747=VECTOR('',#6080,1.);
#748=VECTOR('',#6083,1.);
#749=VECTOR('',#6084,1.);
#750=VECTOR('',#6085,1.);
#751=VECTOR('',#6088,1.);
#752=VECTOR('',#6089,1.);
#753=VECTOR('',#6118,1.);
#754=VECTOR('',#6119,1.);
#755=VECTOR('',#6124,1.);
#756=VECTOR('',#6125,1.);
#757=VECTOR('',#6130,1.);
#758=VECTOR('',#6133,1.);
#759=VECTOR('',#6138,1.2);
#760=VECTOR('',#6141,1.);
#761=VECTOR('',#6144,1.);
#762=VECTOR('',#6149,0.9);
#763=VECTOR('',#6158,0.9);
#764=VECTOR('',#6171,0.9);
#765=VECTOR('',#6180,0.9);
#766=VECTOR('',#6189,0.425);
#767=VECTOR('',#6196,0.425);
#768=VECTOR('',#6203,0.425);
#769=VECTOR('',#6208,1.);
#770=VECTOR('',#6213,1.);
#771=VECTOR('',#6214,1.);
#772=VECTOR('',#6215,1.);
#773=VECTOR('',#6216,1.);
#774=VECTOR('',#6219,1.);
#775=VECTOR('',#6220,1.);
#776=VECTOR('',#6221,1.);
#777=VECTOR('',#6224,1.);
#778=VECTOR('',#6225,1.);
#779=VECTOR('',#6226,1.);
#780=VECTOR('',#6229,1.);
#781=VECTOR('',#6230,1.);
#782=VECTOR('',#6231,1.);
#783=VECTOR('',#6234,1.);
#784=VECTOR('',#6235,1.);
#785=VECTOR('',#6236,1.);
#786=VECTOR('',#6239,1.);
#787=VECTOR('',#6240,1.);
#788=VECTOR('',#6241,1.);
#789=VECTOR('',#6244,1.);
#790=VECTOR('',#6245,1.);
#791=VECTOR('',#6246,1.);
#792=VECTOR('',#6249,1.);
#793=VECTOR('',#6250,1.);
#794=VECTOR('',#6261,1.1);
#795=VECTOR('',#6268,0.425);
#796=VECTOR('',#6275,0.425);
#797=VECTOR('',#6280,1.);
#798=VECTOR('',#6281,1.);
#799=VECTOR('',#6282,1.);
#800=VECTOR('',#6283,1.);
#801=VECTOR('',#6286,1.);
#802=VECTOR('',#6287,1.);
#803=VECTOR('',#6288,1.);
#804=VECTOR('',#6291,1.);
#805=VECTOR('',#6292,1.);
#806=VECTOR('',#6293,1.);
#807=VECTOR('',#6296,1.);
#808=VECTOR('',#6297,1.);
#809=VECTOR('',#6308,0.425);
#810=VECTOR('',#6315,1.);
#811=VECTOR('',#6328,0.34);
#812=VECTOR('',#6341,1.5);
#813=VECTOR('',#6350,1.);
#814=VECTOR('',#6359,0.425);
#815=VECTOR('',#6366,1.5);
#816=VECTOR('',#6379,1.005);
#817=VECTOR('',#6386,1.4);
#818=VECTOR('',#6399,1.005);
#819=VECTOR('',#6406,1.4);
#820=VECTOR('',#6419,1.005);
#821=VECTOR('',#6426,1.4);
#822=VECTOR('',#6439,0.81);
#823=VECTOR('',#6446,1.1);
#824=VECTOR('',#6459,1.005);
#825=VECTOR('',#6466,1.4);
#826=VECTOR('',#6479,1.005);
#827=VECTOR('',#6486,1.4);
#828=VECTOR('',#6497,1.);
#829=VECTOR('',#6498,1.);
#830=VECTOR('',#6499,1.);
#831=VECTOR('',#6500,1.);
#832=VECTOR('',#6503,1.);
#833=VECTOR('',#6504,1.);
#834=VECTOR('',#6505,1.);
#835=VECTOR('',#6508,1.);
#836=VECTOR('',#6509,1.);
#837=VECTOR('',#6510,1.);
#838=VECTOR('',#6513,1.);
#839=VECTOR('',#6514,1.);
#840=VECTOR('',#6515,1.);
#841=VECTOR('',#6518,1.);
#842=VECTOR('',#6519,1.);
#843=VECTOR('',#6520,1.);
#844=VECTOR('',#6523,1.);
#845=VECTOR('',#6524,1.);
#846=VECTOR('',#6537,0.4);
#847=VECTOR('',#6550,0.625);
#848=VECTOR('',#6555,0.65);
#849=VECTOR('',#6560,0.635);
#850=VECTOR('',#6569,0.41);
#851=VECTOR('',#6572,0.4);
#852=VECTOR('',#6579,0.42);
#853=VECTOR('',#6586,0.8);
#854=VECTOR('',#6597,0.734027674973257);
#855=VECTOR('',#6604,0.734027674973257);
#856=VECTOR('',#6607,1.);
#857=VECTOR('',#6608,1.);
#858=VECTOR('',#6611,1.);
#859=VECTOR('',#6614,1.);
#860=VECTOR('',#6619,0.4);
#861=VECTOR('',#6624,1.);
#862=VECTOR('',#6627,1.);
#863=VECTOR('',#6644,0.625);
#864=VECTOR('',#6649,0.65);
#865=VECTOR('',#6654,0.635);
#866=VECTOR('',#6663,0.41);
#867=VECTOR('',#6668,0.4);
#868=VECTOR('',#6673,0.36);
#869=VECTOR('',#6678,1.);
#870=VECTOR('',#6679,1.);
#871=VECTOR('',#6680,1.);
#872=VECTOR('',#6681,1.);
#873=VECTOR('',#6684,1.);
#874=VECTOR('',#6685,1.);
#875=VECTOR('',#6686,1.);
#876=VECTOR('',#6689,1.);
#877=VECTOR('',#6690,1.);
#878=VECTOR('',#6691,1.);
#879=VECTOR('',#6694,1.);
#880=VECTOR('',#6695,1.);
#881=VECTOR('',#6696,1.);
#882=VECTOR('',#6699,1.);
#883=VECTOR('',#6700,1.);
#884=VECTOR('',#6701,1.);
#885=VECTOR('',#6704,1.);
#886=VECTOR('',#6705,1.);
#887=VECTOR('',#6768,0.165);
#888=VECTOR('',#6775,0.165);
#889=VECTOR('',#6782,0.165);
#890=VECTOR('',#6789,0.165);
#891=VECTOR('',#6796,4.7);
#892=VECTOR('',#6803,4.7);
#893=VECTOR('',#6808,5.);
#894=VECTOR('',#6821,5.);
#895=VECTOR('',#6824,3.);
#896=VECTOR('',#6831,2.35);
#897=VECTOR('',#6838,3.);
#898=VECTOR('',#6849,1.9);
#899=VECTOR('',#6856,2.34);
#900=VECTOR('',#6869,0.225);
#901=VECTOR('',#6876,0.225);
#902=VECTOR('',#6883,0.225);
#903=VECTOR('',#6890,0.225);
#904=VECTOR('',#6897,2.34);
#905=VECTOR('',#6906,1.9);
#906=VECTOR('',#6913,3.);
#907=VECTOR('',#6926,0.225);
#908=VECTOR('',#6933,0.225);
#909=VECTOR('',#6940,0.225);
#910=VECTOR('',#6947,0.225);
#911=VECTOR('',#6954,2.34);
#912=VECTOR('',#6965,1.9);
#913=VECTOR('',#6970,3.);
#914=VECTOR('',#6995,1.63531);
#915=VECTOR('',#7002,1.);
#916=VECTOR('',#7007,1.05);
#917=VECTOR('',#7016,1.63531);
#918=VECTOR('',#7023,1.05);
#919=VECTOR('',#7042,1.71469);
#920=VECTOR('',#7053,2.3);
#921=VECTOR('',#7058,2.35);
#922=VECTOR('',#7063,2.3);
#923=VECTOR('',#7068,1.71469);
#924=VECTOR('',#7119,1.706752);
#925=VECTOR('',#7196,1.643248);
#926=VECTOR('',#7225,1.70469);
#927=VECTOR('',#7232,1.65031);
#928=VECTOR('',#7243,1.70469);
#929=VECTOR('',#7250,1.65031);
#930=VECTOR('',#7265,1.);
#931=VECTOR('',#7266,1.);
#932=VECTOR('',#7267,1.);
#933=VECTOR('',#7268,1.);
#934=VECTOR('',#7271,1.);
#935=VECTOR('',#7272,1.);
#936=VECTOR('',#7273,1.);
#937=VECTOR('',#7276,1.);
#938=VECTOR('',#7277,1.);
#939=VECTOR('',#7278,1.);
#940=VECTOR('',#7281,1.);
#941=VECTOR('',#7282,1.);
#942=VECTOR('',#7283,1.);
#943=VECTOR('',#7286,1.);
#944=VECTOR('',#7287,1.);
#945=VECTOR('',#7288,1.);
#946=VECTOR('',#7291,1.);
#947=VECTOR('',#7292,1.);
#948=VECTOR('',#7309,0.325);
#949=VECTOR('',#7314,0.35);
#950=VECTOR('',#7319,0.335);
#951=VECTOR('',#7328,0.21);
#952=VECTOR('',#7331,0.2);
#953=VECTOR('',#7378,1.3);
#954=VECTOR('',#7381,0.8);
#955=VECTOR('',#7392,0.8);
#956=VECTOR('',#7397,1.);
#957=VECTOR('',#7398,1.);
#958=VECTOR('',#7399,1.);
#959=VECTOR('',#7402,1.);
#960=VECTOR('',#7403,1.);
#961=VECTOR('',#7404,1.);
#962=VECTOR('',#7407,1.);
#963=VECTOR('',#7408,1.);
#964=VECTOR('',#7409,1.);
#965=VECTOR('',#7412,1.);
#966=VECTOR('',#7413,1.);
#967=VECTOR('',#7414,1.);
#968=VECTOR('',#7415,1.);
#969=VECTOR('',#7418,1.);
#970=VECTOR('',#7421,1.);
#971=VECTOR('',#7428,1.);
#972=VECTOR('',#7431,1.);
#973=VECTOR('',#7434,1.);
#974=VECTOR('',#7439,1.);
#975=VECTOR('',#7448,0.81);
#976=VECTOR('',#7455,1.5);
#977=VECTOR('',#7468,0.7);
#978=VECTOR('',#7473,1.);
#979=VECTOR('',#7474,1.);
#980=VECTOR('',#7475,1.);
#981=VECTOR('',#7476,1.);
#982=VECTOR('',#7479,1.);
#983=VECTOR('',#7480,1.);
#984=VECTOR('',#7481,1.);
#985=VECTOR('',#7484,1.);
#986=VECTOR('',#7485,1.);
#987=VECTOR('',#7486,1.);
#988=VECTOR('',#7489,1.);
#989=VECTOR('',#7490,1.);
#990=VECTOR('',#7491,1.);
#991=VECTOR('',#7494,1.);
#992=VECTOR('',#7495,1.);
#993=VECTOR('',#7496,1.);
#994=VECTOR('',#7499,1.);
#995=VECTOR('',#7500,1.);
#996=VECTOR('',#7519,1.);
#997=VECTOR('',#7526,1.);
#998=VECTOR('',#7531,1.);
#999=VECTOR('',#7534,1.);
#1000=CYLINDRICAL_SURFACE('',#5272,3.25);
#1001=CYLINDRICAL_SURFACE('',#5274,3.25);
#1002=CYLINDRICAL_SURFACE('',#5276,3.25);
#1003=CYLINDRICAL_SURFACE('',#5278,1.2);
#1004=CYLINDRICAL_SURFACE('',#5280,3.25);
#1005=CYLINDRICAL_SURFACE('',#5282,0.9);
#1006=CYLINDRICAL_SURFACE('',#5286,0.9);
#1007=CYLINDRICAL_SURFACE('',#5290,0.9);
#1008=CYLINDRICAL_SURFACE('',#5296,0.9);
#1009=CYLINDRICAL_SURFACE('',#5300,0.425);
#1010=CYLINDRICAL_SURFACE('',#5303,0.425);
#1011=CYLINDRICAL_SURFACE('',#5306,0.425);
#1012=CYLINDRICAL_SURFACE('',#5309,1.);
#1013=CYLINDRICAL_SURFACE('',#5332,3.25);
#1014=CYLINDRICAL_SURFACE('',#5334,3.25);
#1015=CYLINDRICAL_SURFACE('',#5336,3.25);
#1016=CYLINDRICAL_SURFACE('',#5338,1.2);
#1017=CYLINDRICAL_SURFACE('',#5340,3.25);
#1018=CYLINDRICAL_SURFACE('',#5342,0.9);
#1019=CYLINDRICAL_SURFACE('',#5346,0.9);
#1020=CYLINDRICAL_SURFACE('',#5352,0.9);
#1021=CYLINDRICAL_SURFACE('',#5356,0.9);
#1022=CYLINDRICAL_SURFACE('',#5360,0.425);
#1023=CYLINDRICAL_SURFACE('',#5363,0.425);
#1024=CYLINDRICAL_SURFACE('',#5366,0.425);
#1025=CYLINDRICAL_SURFACE('',#5369,1.);
#1026=CYLINDRICAL_SURFACE('',#5382,1.1);
#1027=CYLINDRICAL_SURFACE('',#5385,0.425);
#1028=CYLINDRICAL_SURFACE('',#5388,0.425);
#1029=CYLINDRICAL_SURFACE('',#5398,0.425);
#1030=CYLINDRICAL_SURFACE('',#5401,1.);
#1031=CYLINDRICAL_SURFACE('',#5407,0.34);
#1032=CYLINDRICAL_SURFACE('',#5414,1.5);
#1033=CYLINDRICAL_SURFACE('',#5417,1.);
#1034=CYLINDRICAL_SURFACE('',#5421,0.425);
#1035=CYLINDRICAL_SURFACE('',#5424,1.5);
#1036=CYLINDRICAL_SURFACE('',#5430,1.005);
#1037=CYLINDRICAL_SURFACE('',#5433,1.4);
#1038=CYLINDRICAL_SURFACE('',#5439,1.005);
#1039=CYLINDRICAL_SURFACE('',#5442,1.4);
#1040=CYLINDRICAL_SURFACE('',#5448,1.005);
#1041=CYLINDRICAL_SURFACE('',#5451,1.4);
#1042=CYLINDRICAL_SURFACE('',#5457,0.81);
#1043=CYLINDRICAL_SURFACE('',#5460,1.1);
#1044=CYLINDRICAL_SURFACE('',#5466,1.005);
#1045=CYLINDRICAL_SURFACE('',#5469,1.4);
#1046=CYLINDRICAL_SURFACE('',#5475,1.005);
#1047=CYLINDRICAL_SURFACE('',#5478,1.4);
#1048=CYLINDRICAL_SURFACE('',#5495,0.4);
#1049=CYLINDRICAL_SURFACE('',#5502,0.65);
#1050=CYLINDRICAL_SURFACE('',#5510,0.3933);
#1051=CYLINDRICAL_SURFACE('',#5512,0.42);
#1052=CYLINDRICAL_SURFACE('',#5515,0.8);
#1053=CYLINDRICAL_SURFACE('',#5528,0.338975);
#1054=CYLINDRICAL_SURFACE('',#5541,0.65);
#1055=CYLINDRICAL_SURFACE('',#5549,0.3933);
#1056=CYLINDRICAL_SURFACE('',#5589,0.165);
#1057=CYLINDRICAL_SURFACE('',#5592,0.165);
#1058=CYLINDRICAL_SURFACE('',#5595,0.165);
#1059=CYLINDRICAL_SURFACE('',#5598,0.165);
#1060=CYLINDRICAL_SURFACE('',#5606,5.);
#1061=CYLINDRICAL_SURFACE('',#5613,5.);
#1062=CYLINDRICAL_SURFACE('',#5614,3.);
#1063=CYLINDRICAL_SURFACE('',#5616,2.35);
#1064=CYLINDRICAL_SURFACE('',#5619,3.);
#1065=CYLINDRICAL_SURFACE('',#5624,1.9);
#1066=CYLINDRICAL_SURFACE('',#5627,2.34);
#1067=CYLINDRICAL_SURFACE('',#5633,0.225);
#1068=CYLINDRICAL_SURFACE('',#5636,0.225);
#1069=CYLINDRICAL_SURFACE('',#5639,0.225);
#1070=CYLINDRICAL_SURFACE('',#5642,0.225);
#1071=CYLINDRICAL_SURFACE('',#5645,2.34);
#1072=CYLINDRICAL_SURFACE('',#5650,1.9);
#1073=CYLINDRICAL_SURFACE('',#5652,3.);
#1074=CYLINDRICAL_SURFACE('',#5658,0.225);
#1075=CYLINDRICAL_SURFACE('',#5661,0.225);
#1076=CYLINDRICAL_SURFACE('',#5664,0.225);
#1077=CYLINDRICAL_SURFACE('',#5667,0.225);
#1078=CYLINDRICAL_SURFACE('',#5670,2.34);
#1079=CYLINDRICAL_SURFACE('',#5675,1.9);
#1080=CYLINDRICAL_SURFACE('',#5677,3.);
#1081=CYLINDRICAL_SURFACE('',#5690,1.63531);
#1082=CYLINDRICAL_SURFACE('',#5692,1.);
#1083=CYLINDRICAL_SURFACE('',#5698,1.63531);
#1084=CYLINDRICAL_SURFACE('',#5710,1.71469);
#1085=CYLINDRICAL_SURFACE('',#5717,2.35);
#1086=CYLINDRICAL_SURFACE('',#5722,1.71469);
#1087=CYLINDRICAL_SURFACE('',#5744,1.706752);
#1088=CYLINDRICAL_SURFACE('',#5784,1.643248);
#1089=CYLINDRICAL_SURFACE('',#5798,1.70469);
#1090=CYLINDRICAL_SURFACE('',#5802,1.65031);
#1091=CYLINDRICAL_SURFACE('',#5806,1.70469);
#1092=CYLINDRICAL_SURFACE('',#5810,1.65031);
#1093=CYLINDRICAL_SURFACE('',#5831,0.35);
#1094=CYLINDRICAL_SURFACE('',#5839,0.1954);
#1095=CYLINDRICAL_SURFACE('',#5862,1.3);
#1096=CYLINDRICAL_SURFACE('',#5863,0.8);
#1097=CYLINDRICAL_SURFACE('',#5867,0.8);
#1098=CYLINDRICAL_SURFACE('',#5877,2.);
#1099=CYLINDRICAL_SURFACE('',#5883,3.5);
#1100=CYLINDRICAL_SURFACE('',#5885,0.81);
#1101=CYLINDRICAL_SURFACE('',#5888,1.5);
#1102=CYLINDRICAL_SURFACE('',#5894,0.7);
#1103=CYLINDRICAL_SURFACE('',#5910,1.);
#1104=CYLINDRICAL_SURFACE('',#5913,1.);
#1105=CYLINDRICAL_SURFACE('',#5916,2.);
#1106=CYLINDRICAL_SURFACE('',#5921,2.);
#1107=FACE_BOUND('',#1512,.T.);
#1108=FACE_BOUND('',#1522,.T.);
#1109=FACE_BOUND('',#1537,.T.);
#1110=FACE_BOUND('',#1538,.T.);
#1111=FACE_BOUND('',#1539,.T.);
#1112=FACE_BOUND('',#1540,.T.);
#1113=FACE_BOUND('',#1542,.T.);
#1114=FACE_BOUND('',#1543,.T.);
#1115=FACE_BOUND('',#1544,.T.);
#1116=FACE_BOUND('',#1545,.T.);
#1117=FACE_BOUND('',#1546,.T.);
#1118=FACE_BOUND('',#1547,.T.);
#1119=FACE_BOUND('',#1548,.T.);
#1120=FACE_BOUND('',#1549,.T.);
#1121=FACE_BOUND('',#1551,.T.);
#1122=FACE_BOUND('',#1560,.T.);
#1123=FACE_BOUND('',#1576,.T.);
#1124=FACE_BOUND('',#1577,.T.);
#1125=FACE_BOUND('',#1578,.T.);
#1126=FACE_BOUND('',#1579,.T.);
#1127=FACE_BOUND('',#1580,.T.);
#1128=FACE_BOUND('',#1581,.T.);
#1129=FACE_BOUND('',#1582,.T.);
#1130=FACE_BOUND('',#1583,.T.);
#1131=FACE_BOUND('',#1585,.T.);
#1132=FACE_BOUND('',#1586,.T.);
#1133=FACE_BOUND('',#1587,.T.);
#1134=FACE_BOUND('',#1588,.T.);
#1135=FACE_BOUND('',#1593,.T.);
#1136=FACE_BOUND('',#1594,.T.);
#1137=FACE_BOUND('',#1597,.T.);
#1138=FACE_BOUND('',#1598,.T.);
#1139=FACE_BOUND('',#1601,.T.);
#1140=FACE_BOUND('',#1603,.T.);
#1141=FACE_BOUND('',#1607,.T.);
#1142=FACE_BOUND('',#1609,.T.);
#1143=FACE_BOUND('',#1613,.T.);
#1144=FACE_BOUND('',#1618,.T.);
#1145=FACE_BOUND('',#1622,.T.);
#1146=FACE_BOUND('',#1624,.T.);
#1147=FACE_BOUND('',#1628,.T.);
#1148=FACE_BOUND('',#1630,.T.);
#1149=FACE_BOUND('',#1634,.T.);
#1150=FACE_BOUND('',#1636,.T.);
#1151=FACE_BOUND('',#1640,.T.);
#1152=FACE_BOUND('',#1642,.T.);
#1153=FACE_BOUND('',#1646,.T.);
#1154=FACE_BOUND('',#1648,.T.);
#1155=FACE_BOUND('',#1652,.T.);
#1156=FACE_BOUND('',#1654,.T.);
#1157=FACE_BOUND('',#1658,.T.);
#1158=FACE_BOUND('',#1660,.T.);
#1159=FACE_BOUND('',#1670,.T.);
#1160=FACE_BOUND('',#1678,.T.);
#1161=FACE_BOUND('',#1684,.T.);
#1162=FACE_BOUND('',#1686,.T.);
#1163=FACE_BOUND('',#1697,.T.);
#1164=FACE_BOUND('',#1699,.T.);
#1165=FACE_BOUND('',#1705,.T.);
#1166=FACE_BOUND('',#1726,.T.);
#1167=FACE_BOUND('',#1728,.T.);
#1168=FACE_BOUND('',#1734,.T.);
#1169=FACE_BOUND('',#1735,.T.);
#1170=FACE_BOUND('',#1736,.T.);
#1171=FACE_BOUND('',#1737,.T.);
#1172=FACE_BOUND('',#1738,.T.);
#1173=FACE_BOUND('',#1740,.T.);
#1174=FACE_BOUND('',#1741,.T.);
#1175=FACE_BOUND('',#1742,.T.);
#1176=FACE_BOUND('',#1743,.T.);
#1177=FACE_BOUND('',#1744,.T.);
#1178=FACE_BOUND('',#1748,.T.);
#1179=FACE_BOUND('',#1750,.T.);
#1180=FACE_BOUND('',#1757,.T.);
#1181=FACE_BOUND('',#1761,.T.);
#1182=FACE_BOUND('',#1762,.T.);
#1183=FACE_BOUND('',#1763,.T.);
#1184=FACE_BOUND('',#1764,.T.);
#1185=FACE_BOUND('',#1765,.T.);
#1186=FACE_BOUND('',#1767,.T.);
#1187=FACE_BOUND('',#1768,.T.);
#1188=FACE_BOUND('',#1769,.T.);
#1189=FACE_BOUND('',#1770,.T.);
#1190=FACE_BOUND('',#1771,.T.);
#1191=FACE_BOUND('',#1778,.T.);
#1192=FACE_BOUND('',#1782,.T.);
#1193=FACE_BOUND('',#1783,.T.);
#1194=FACE_BOUND('',#1784,.T.);
#1195=FACE_BOUND('',#1785,.T.);
#1196=FACE_BOUND('',#1786,.T.);
#1197=FACE_BOUND('',#1788,.T.);
#1198=FACE_BOUND('',#1789,.T.);
#1199=FACE_BOUND('',#1790,.T.);
#1200=FACE_BOUND('',#1791,.T.);
#1201=FACE_BOUND('',#1792,.T.);
#1202=FACE_BOUND('',#1798,.T.);
#1203=FACE_BOUND('',#1801,.T.);
#1204=FACE_BOUND('',#1806,.T.);
#1205=FACE_BOUND('',#1811,.T.);
#1206=FACE_BOUND('',#1839,.T.);
#1207=FACE_BOUND('',#1842,.T.);
#1208=FACE_BOUND('',#1845,.T.);
#1209=FACE_BOUND('',#1848,.T.);
#1210=FACE_BOUND('',#1851,.T.);
#1211=FACE_BOUND('',#1867,.T.);
#1212=FACE_BOUND('',#1871,.T.);
#1213=FACE_BOUND('',#1873,.T.);
#1214=FACE_BOUND('',#1891,.T.);
#1215=FACE_BOUND('',#1893,.T.);
#1216=FACE_BOUND('',#1902,.T.);
#1217=FACE_BOUND('',#1904,.T.);
#1218=FACE_BOUND('',#1909,.T.);
#1219=FACE_BOUND('',#1910,.T.);
#1220=FACE_BOUND('',#1913,.T.);
#1221=FACE_BOUND('',#1914,.T.);
#1222=FACE_OUTER_BOUND('',#1511,.T.);
#1223=FACE_OUTER_BOUND('',#1513,.T.);
#1224=FACE_OUTER_BOUND('',#1514,.T.);
#1225=FACE_OUTER_BOUND('',#1515,.T.);
#1226=FACE_OUTER_BOUND('',#1516,.T.);
#1227=FACE_OUTER_BOUND('',#1517,.T.);
#1228=FACE_OUTER_BOUND('',#1518,.T.);
#1229=FACE_OUTER_BOUND('',#1519,.T.);
#1230=FACE_OUTER_BOUND('',#1520,.T.);
#1231=FACE_OUTER_BOUND('',#1521,.T.);
#1232=FACE_OUTER_BOUND('',#1523,.T.);
#1233=FACE_OUTER_BOUND('',#1524,.T.);
#1234=FACE_OUTER_BOUND('',#1525,.T.);
#1235=FACE_OUTER_BOUND('',#1526,.T.);
#1236=FACE_OUTER_BOUND('',#1527,.T.);
#1237=FACE_OUTER_BOUND('',#1528,.T.);
#1238=FACE_OUTER_BOUND('',#1529,.T.);
#1239=FACE_OUTER_BOUND('',#1530,.T.);
#1240=FACE_OUTER_BOUND('',#1531,.T.);
#1241=FACE_OUTER_BOUND('',#1532,.T.);
#1242=FACE_OUTER_BOUND('',#1533,.T.);
#1243=FACE_OUTER_BOUND('',#1534,.T.);
#1244=FACE_OUTER_BOUND('',#1535,.T.);
#1245=FACE_OUTER_BOUND('',#1536,.T.);
#1246=FACE_OUTER_BOUND('',#1541,.T.);
#1247=FACE_OUTER_BOUND('',#1550,.T.);
#1248=FACE_OUTER_BOUND('',#1552,.T.);
#1249=FACE_OUTER_BOUND('',#1553,.T.);
#1250=FACE_OUTER_BOUND('',#1554,.T.);
#1251=FACE_OUTER_BOUND('',#1555,.T.);
#1252=FACE_OUTER_BOUND('',#1556,.T.);
#1253=FACE_OUTER_BOUND('',#1557,.T.);
#1254=FACE_OUTER_BOUND('',#1558,.T.);
#1255=FACE_OUTER_BOUND('',#1559,.T.);
#1256=FACE_OUTER_BOUND('',#1561,.T.);
#1257=FACE_OUTER_BOUND('',#1562,.T.);
#1258=FACE_OUTER_BOUND('',#1563,.T.);
#1259=FACE_OUTER_BOUND('',#1564,.T.);
#1260=FACE_OUTER_BOUND('',#1565,.T.);
#1261=FACE_OUTER_BOUND('',#1566,.T.);
#1262=FACE_OUTER_BOUND('',#1567,.T.);
#1263=FACE_OUTER_BOUND('',#1568,.T.);
#1264=FACE_OUTER_BOUND('',#1569,.T.);
#1265=FACE_OUTER_BOUND('',#1570,.T.);
#1266=FACE_OUTER_BOUND('',#1571,.T.);
#1267=FACE_OUTER_BOUND('',#1572,.T.);
#1268=FACE_OUTER_BOUND('',#1573,.T.);
#1269=FACE_OUTER_BOUND('',#1574,.T.);
#1270=FACE_OUTER_BOUND('',#1575,.T.);
#1271=FACE_OUTER_BOUND('',#1584,.T.);
#1272=FACE_OUTER_BOUND('',#1589,.T.);
#1273=FACE_OUTER_BOUND('',#1590,.T.);
#1274=FACE_OUTER_BOUND('',#1591,.T.);
#1275=FACE_OUTER_BOUND('',#1592,.T.);
#1276=FACE_OUTER_BOUND('',#1595,.T.);
#1277=FACE_OUTER_BOUND('',#1596,.T.);
#1278=FACE_OUTER_BOUND('',#1599,.T.);
#1279=FACE_OUTER_BOUND('',#1600,.T.);
#1280=FACE_OUTER_BOUND('',#1602,.T.);
#1281=FACE_OUTER_BOUND('',#1604,.T.);
#1282=FACE_OUTER_BOUND('',#1605,.T.);
#1283=FACE_OUTER_BOUND('',#1606,.T.);
#1284=FACE_OUTER_BOUND('',#1608,.T.);
#1285=FACE_OUTER_BOUND('',#1610,.T.);
#1286=FACE_OUTER_BOUND('',#1611,.T.);
#1287=FACE_OUTER_BOUND('',#1612,.T.);
#1288=FACE_OUTER_BOUND('',#1614,.T.);
#1289=FACE_OUTER_BOUND('',#1615,.T.);
#1290=FACE_OUTER_BOUND('',#1616,.T.);
#1291=FACE_OUTER_BOUND('',#1617,.T.);
#1292=FACE_OUTER_BOUND('',#1619,.T.);
#1293=FACE_OUTER_BOUND('',#1620,.T.);
#1294=FACE_OUTER_BOUND('',#1621,.T.);
#1295=FACE_OUTER_BOUND('',#1623,.T.);
#1296=FACE_OUTER_BOUND('',#1625,.T.);
#1297=FACE_OUTER_BOUND('',#1626,.T.);
#1298=FACE_OUTER_BOUND('',#1627,.T.);
#1299=FACE_OUTER_BOUND('',#1629,.T.);
#1300=FACE_OUTER_BOUND('',#1631,.T.);
#1301=FACE_OUTER_BOUND('',#1632,.T.);
#1302=FACE_OUTER_BOUND('',#1633,.T.);
#1303=FACE_OUTER_BOUND('',#1635,.T.);
#1304=FACE_OUTER_BOUND('',#1637,.T.);
#1305=FACE_OUTER_BOUND('',#1638,.T.);
#1306=FACE_OUTER_BOUND('',#1639,.T.);
#1307=FACE_OUTER_BOUND('',#1641,.T.);
#1308=FACE_OUTER_BOUND('',#1643,.T.);
#1309=FACE_OUTER_BOUND('',#1644,.T.);
#1310=FACE_OUTER_BOUND('',#1645,.T.);
#1311=FACE_OUTER_BOUND('',#1647,.T.);
#1312=FACE_OUTER_BOUND('',#1649,.T.);
#1313=FACE_OUTER_BOUND('',#1650,.T.);
#1314=FACE_OUTER_BOUND('',#1651,.T.);
#1315=FACE_OUTER_BOUND('',#1653,.T.);
#1316=FACE_OUTER_BOUND('',#1655,.T.);
#1317=FACE_OUTER_BOUND('',#1656,.T.);
#1318=FACE_OUTER_BOUND('',#1657,.T.);
#1319=FACE_OUTER_BOUND('',#1659,.T.);
#1320=FACE_OUTER_BOUND('',#1661,.T.);
#1321=FACE_OUTER_BOUND('',#1662,.T.);
#1322=FACE_OUTER_BOUND('',#1663,.T.);
#1323=FACE_OUTER_BOUND('',#1664,.T.);
#1324=FACE_OUTER_BOUND('',#1665,.T.);
#1325=FACE_OUTER_BOUND('',#1666,.T.);
#1326=FACE_OUTER_BOUND('',#1667,.T.);
#1327=FACE_OUTER_BOUND('',#1668,.T.);
#1328=FACE_OUTER_BOUND('',#1669,.T.);
#1329=FACE_OUTER_BOUND('',#1671,.T.);
#1330=FACE_OUTER_BOUND('',#1672,.T.);
#1331=FACE_OUTER_BOUND('',#1673,.T.);
#1332=FACE_OUTER_BOUND('',#1674,.T.);
#1333=FACE_OUTER_BOUND('',#1675,.T.);
#1334=FACE_OUTER_BOUND('',#1676,.T.);
#1335=FACE_OUTER_BOUND('',#1677,.T.);
#1336=FACE_OUTER_BOUND('',#1679,.T.);
#1337=FACE_OUTER_BOUND('',#1680,.T.);
#1338=FACE_OUTER_BOUND('',#1681,.T.);
#1339=FACE_OUTER_BOUND('',#1682,.T.);
#1340=FACE_OUTER_BOUND('',#1683,.T.);
#1341=FACE_OUTER_BOUND('',#1685,.T.);
#1342=FACE_OUTER_BOUND('',#1687,.T.);
#1343=FACE_OUTER_BOUND('',#1688,.T.);
#1344=FACE_OUTER_BOUND('',#1689,.T.);
#1345=FACE_OUTER_BOUND('',#1690,.T.);
#1346=FACE_OUTER_BOUND('',#1691,.T.);
#1347=FACE_OUTER_BOUND('',#1692,.T.);
#1348=FACE_OUTER_BOUND('',#1693,.T.);
#1349=FACE_OUTER_BOUND('',#1694,.T.);
#1350=FACE_OUTER_BOUND('',#1695,.T.);
#1351=FACE_OUTER_BOUND('',#1696,.T.);
#1352=FACE_OUTER_BOUND('',#1698,.T.);
#1353=FACE_OUTER_BOUND('',#1700,.T.);
#1354=FACE_OUTER_BOUND('',#1701,.T.);
#1355=FACE_OUTER_BOUND('',#1702,.T.);
#1356=FACE_OUTER_BOUND('',#1703,.T.);
#1357=FACE_OUTER_BOUND('',#1704,.T.);
#1358=FACE_OUTER_BOUND('',#1706,.T.);
#1359=FACE_OUTER_BOUND('',#1707,.T.);
#1360=FACE_OUTER_BOUND('',#1708,.T.);
#1361=FACE_OUTER_BOUND('',#1709,.T.);
#1362=FACE_OUTER_BOUND('',#1710,.T.);
#1363=FACE_OUTER_BOUND('',#1711,.T.);
#1364=FACE_OUTER_BOUND('',#1712,.T.);
#1365=FACE_OUTER_BOUND('',#1713,.T.);
#1366=FACE_OUTER_BOUND('',#1714,.T.);
#1367=FACE_OUTER_BOUND('',#1715,.T.);
#1368=FACE_OUTER_BOUND('',#1716,.T.);
#1369=FACE_OUTER_BOUND('',#1717,.T.);
#1370=FACE_OUTER_BOUND('',#1718,.T.);
#1371=FACE_OUTER_BOUND('',#1719,.T.);
#1372=FACE_OUTER_BOUND('',#1720,.T.);
#1373=FACE_OUTER_BOUND('',#1721,.T.);
#1374=FACE_OUTER_BOUND('',#1722,.T.);
#1375=FACE_OUTER_BOUND('',#1723,.T.);
#1376=FACE_OUTER_BOUND('',#1724,.T.);
#1377=FACE_OUTER_BOUND('',#1725,.T.);
#1378=FACE_OUTER_BOUND('',#1727,.T.);
#1379=FACE_OUTER_BOUND('',#1729,.T.);
#1380=FACE_OUTER_BOUND('',#1730,.T.);
#1381=FACE_OUTER_BOUND('',#1731,.T.);
#1382=FACE_OUTER_BOUND('',#1732,.T.);
#1383=FACE_OUTER_BOUND('',#1733,.T.);
#1384=FACE_OUTER_BOUND('',#1739,.T.);
#1385=FACE_OUTER_BOUND('',#1745,.T.);
#1386=FACE_OUTER_BOUND('',#1746,.T.);
#1387=FACE_OUTER_BOUND('',#1747,.T.);
#1388=FACE_OUTER_BOUND('',#1749,.T.);
#1389=FACE_OUTER_BOUND('',#1751,.T.);
#1390=FACE_OUTER_BOUND('',#1752,.T.);
#1391=FACE_OUTER_BOUND('',#1753,.T.);
#1392=FACE_OUTER_BOUND('',#1754,.T.);
#1393=FACE_OUTER_BOUND('',#1755,.T.);
#1394=FACE_OUTER_BOUND('',#1756,.T.);
#1395=FACE_OUTER_BOUND('',#1758,.T.);
#1396=FACE_OUTER_BOUND('',#1759,.T.);
#1397=FACE_OUTER_BOUND('',#1760,.T.);
#1398=FACE_OUTER_BOUND('',#1766,.T.);
#1399=FACE_OUTER_BOUND('',#1772,.T.);
#1400=FACE_OUTER_BOUND('',#1773,.T.);
#1401=FACE_OUTER_BOUND('',#1774,.T.);
#1402=FACE_OUTER_BOUND('',#1775,.T.);
#1403=FACE_OUTER_BOUND('',#1776,.T.);
#1404=FACE_OUTER_BOUND('',#1777,.T.);
#1405=FACE_OUTER_BOUND('',#1779,.T.);
#1406=FACE_OUTER_BOUND('',#1780,.T.);
#1407=FACE_OUTER_BOUND('',#1781,.T.);
#1408=FACE_OUTER_BOUND('',#1787,.T.);
#1409=FACE_OUTER_BOUND('',#1793,.T.);
#1410=FACE_OUTER_BOUND('',#1794,.T.);
#1411=FACE_OUTER_BOUND('',#1795,.T.);
#1412=FACE_OUTER_BOUND('',#1796,.T.);
#1413=FACE_OUTER_BOUND('',#1797,.T.);
#1414=FACE_OUTER_BOUND('',#1799,.T.);
#1415=FACE_OUTER_BOUND('',#1800,.T.);
#1416=FACE_OUTER_BOUND('',#1802,.T.);
#1417=FACE_OUTER_BOUND('',#1803,.T.);
#1418=FACE_OUTER_BOUND('',#1804,.T.);
#1419=FACE_OUTER_BOUND('',#1805,.T.);
#1420=FACE_OUTER_BOUND('',#1807,.T.);
#1421=FACE_OUTER_BOUND('',#1808,.T.);
#1422=FACE_OUTER_BOUND('',#1809,.T.);
#1423=FACE_OUTER_BOUND('',#1810,.T.);
#1424=FACE_OUTER_BOUND('',#1812,.T.);
#1425=FACE_OUTER_BOUND('',#1813,.T.);
#1426=FACE_OUTER_BOUND('',#1814,.T.);
#1427=FACE_OUTER_BOUND('',#1815,.T.);
#1428=FACE_OUTER_BOUND('',#1816,.T.);
#1429=FACE_OUTER_BOUND('',#1817,.T.);
#1430=FACE_OUTER_BOUND('',#1818,.T.);
#1431=FACE_OUTER_BOUND('',#1819,.T.);
#1432=FACE_OUTER_BOUND('',#1820,.T.);
#1433=FACE_OUTER_BOUND('',#1821,.T.);
#1434=FACE_OUTER_BOUND('',#1822,.T.);
#1435=FACE_OUTER_BOUND('',#1823,.T.);
#1436=FACE_OUTER_BOUND('',#1824,.T.);
#1437=FACE_OUTER_BOUND('',#1825,.T.);
#1438=FACE_OUTER_BOUND('',#1826,.T.);
#1439=FACE_OUTER_BOUND('',#1827,.T.);
#1440=FACE_OUTER_BOUND('',#1828,.T.);
#1441=FACE_OUTER_BOUND('',#1829,.T.);
#1442=FACE_OUTER_BOUND('',#1830,.T.);
#1443=FACE_OUTER_BOUND('',#1831,.T.);
#1444=FACE_OUTER_BOUND('',#1832,.T.);
#1445=FACE_OUTER_BOUND('',#1833,.T.);
#1446=FACE_OUTER_BOUND('',#1834,.T.);
#1447=FACE_OUTER_BOUND('',#1835,.T.);
#1448=FACE_OUTER_BOUND('',#1836,.T.);
#1449=FACE_OUTER_BOUND('',#1837,.T.);
#1450=FACE_OUTER_BOUND('',#1838,.T.);
#1451=FACE_OUTER_BOUND('',#1840,.T.);
#1452=FACE_OUTER_BOUND('',#1841,.T.);
#1453=FACE_OUTER_BOUND('',#1843,.T.);
#1454=FACE_OUTER_BOUND('',#1844,.T.);
#1455=FACE_OUTER_BOUND('',#1846,.T.);
#1456=FACE_OUTER_BOUND('',#1847,.T.);
#1457=FACE_OUTER_BOUND('',#1849,.T.);
#1458=FACE_OUTER_BOUND('',#1850,.T.);
#1459=FACE_OUTER_BOUND('',#1852,.T.);
#1460=FACE_OUTER_BOUND('',#1853,.T.);
#1461=FACE_OUTER_BOUND('',#1854,.T.);
#1462=FACE_OUTER_BOUND('',#1855,.T.);
#1463=FACE_OUTER_BOUND('',#1856,.T.);
#1464=FACE_OUTER_BOUND('',#1857,.T.);
#1465=FACE_OUTER_BOUND('',#1858,.T.);
#1466=FACE_OUTER_BOUND('',#1859,.T.);
#1467=FACE_OUTER_BOUND('',#1860,.T.);
#1468=FACE_OUTER_BOUND('',#1861,.T.);
#1469=FACE_OUTER_BOUND('',#1862,.T.);
#1470=FACE_OUTER_BOUND('',#1863,.T.);
#1471=FACE_OUTER_BOUND('',#1864,.T.);
#1472=FACE_OUTER_BOUND('',#1865,.T.);
#1473=FACE_OUTER_BOUND('',#1866,.T.);
#1474=FACE_OUTER_BOUND('',#1868,.T.);
#1475=FACE_OUTER_BOUND('',#1869,.T.);
#1476=FACE_OUTER_BOUND('',#1870,.T.);
#1477=FACE_OUTER_BOUND('',#1872,.T.);
#1478=FACE_OUTER_BOUND('',#1874,.T.);
#1479=FACE_OUTER_BOUND('',#1875,.T.);
#1480=FACE_OUTER_BOUND('',#1876,.T.);
#1481=FACE_OUTER_BOUND('',#1877,.T.);
#1482=FACE_OUTER_BOUND('',#1878,.T.);
#1483=FACE_OUTER_BOUND('',#1879,.T.);
#1484=FACE_OUTER_BOUND('',#1880,.T.);
#1485=FACE_OUTER_BOUND('',#1881,.T.);
#1486=FACE_OUTER_BOUND('',#1882,.T.);
#1487=FACE_OUTER_BOUND('',#1883,.T.);
#1488=FACE_OUTER_BOUND('',#1884,.T.);
#1489=FACE_OUTER_BOUND('',#1885,.T.);
#1490=FACE_OUTER_BOUND('',#1886,.T.);
#1491=FACE_OUTER_BOUND('',#1887,.T.);
#1492=FACE_OUTER_BOUND('',#1888,.T.);
#1493=FACE_OUTER_BOUND('',#1889,.T.);
#1494=FACE_OUTER_BOUND('',#1890,.T.);
#1495=FACE_OUTER_BOUND('',#1892,.T.);
#1496=FACE_OUTER_BOUND('',#1894,.T.);
#1497=FACE_OUTER_BOUND('',#1895,.T.);
#1498=FACE_OUTER_BOUND('',#1896,.T.);
#1499=FACE_OUTER_BOUND('',#1897,.T.);
#1500=FACE_OUTER_BOUND('',#1898,.T.);
#1501=FACE_OUTER_BOUND('',#1899,.T.);
#1502=FACE_OUTER_BOUND('',#1900,.T.);
#1503=FACE_OUTER_BOUND('',#1901,.T.);
#1504=FACE_OUTER_BOUND('',#1903,.T.);
#1505=FACE_OUTER_BOUND('',#1905,.T.);
#1506=FACE_OUTER_BOUND('',#1906,.T.);
#1507=FACE_OUTER_BOUND('',#1907,.T.);
#1508=FACE_OUTER_BOUND('',#1908,.T.);
#1509=FACE_OUTER_BOUND('',#1911,.T.);
#1510=FACE_OUTER_BOUND('',#1912,.T.);
#1511=EDGE_LOOP('',(#3230,#3231,#3232,#3233,#3234,#3235,#3236,#3237));
#1512=EDGE_LOOP('',(#3238));
#1513=EDGE_LOOP('',(#3239,#3240,#3241,#3242));
#1514=EDGE_LOOP('',(#3243,#3244,#3245,#3246));
#1515=EDGE_LOOP('',(#3247,#3248,#3249,#3250));
#1516=EDGE_LOOP('',(#3251,#3252,#3253,#3254));
#1517=EDGE_LOOP('',(#3255,#3256,#3257,#3258));
#1518=EDGE_LOOP('',(#3259,#3260,#3261,#3262,#3263,#3264,#3265,#3266));
#1519=EDGE_LOOP('',(#3267,#3268,#3269,#3270,#3271,#3272,#3273,#3274));
#1520=EDGE_LOOP('',(#3275,#3276,#3277,#3278,#3279,#3280,#3281,#3282));
#1521=EDGE_LOOP('',(#3283));
#1522=EDGE_LOOP('',(#3284));
#1523=EDGE_LOOP('',(#3285,#3286,#3287,#3288,#3289,#3290,#3291,#3292));
#1524=EDGE_LOOP('',(#3293,#3294,#3295,#3296));
#1525=EDGE_LOOP('',(#3297,#3298,#3299,#3300));
#1526=EDGE_LOOP('',(#3301,#3302,#3303,#3304));
#1527=EDGE_LOOP('',(#3305,#3306,#3307,#3308));
#1528=EDGE_LOOP('',(#3309,#3310,#3311,#3312));
#1529=EDGE_LOOP('',(#3313,#3314,#3315,#3316));
#1530=EDGE_LOOP('',(#3317,#3318,#3319,#3320));
#1531=EDGE_LOOP('',(#3321,#3322,#3323,#3324));
#1532=EDGE_LOOP('',(#3325,#3326,#3327,#3328));
#1533=EDGE_LOOP('',(#3329,#3330,#3331,#3332));
#1534=EDGE_LOOP('',(#3333,#3334,#3335,#3336));
#1535=EDGE_LOOP('',(#3337,#3338,#3339,#3340));
#1536=EDGE_LOOP('',(#3341,#3342,#3343,#3344,#3345,#3346,#3347,#3348));
#1537=EDGE_LOOP('',(#3349,#3350,#3351,#3352,#3353,#3354,#3355,#3356,#3357,
#3358,#3359,#3360));
#1538=EDGE_LOOP('',(#3361));
#1539=EDGE_LOOP('',(#3362));
#1540=EDGE_LOOP('',(#3363));
#1541=EDGE_LOOP('',(#3364,#3365,#3366,#3367,#3368,#3369,#3370,#3371));
#1542=EDGE_LOOP('',(#3372));
#1543=EDGE_LOOP('',(#3373));
#1544=EDGE_LOOP('',(#3374));
#1545=EDGE_LOOP('',(#3375));
#1546=EDGE_LOOP('',(#3376));
#1547=EDGE_LOOP('',(#3377));
#1548=EDGE_LOOP('',(#3378));
#1549=EDGE_LOOP('',(#3379));
#1550=EDGE_LOOP('',(#3380,#3381,#3382,#3383,#3384,#3385,#3386,#3387));
#1551=EDGE_LOOP('',(#3388));
#1552=EDGE_LOOP('',(#3389,#3390,#3391,#3392));
#1553=EDGE_LOOP('',(#3393,#3394,#3395,#3396));
#1554=EDGE_LOOP('',(#3397,#3398,#3399,#3400));
#1555=EDGE_LOOP('',(#3401,#3402,#3403,#3404));
#1556=EDGE_LOOP('',(#3405,#3406,#3407,#3408));
#1557=EDGE_LOOP('',(#3409,#3410,#3411,#3412,#3413,#3414,#3415,#3416));
#1558=EDGE_LOOP('',(#3417,#3418,#3419,#3420,#3421,#3422,#3423,#3424));
#1559=EDGE_LOOP('',(#3425));
#1560=EDGE_LOOP('',(#3426));
#1561=EDGE_LOOP('',(#3427,#3428,#3429,#3430,#3431,#3432,#3433,#3434));
#1562=EDGE_LOOP('',(#3435,#3436,#3437,#3438,#3439,#3440,#3441,#3442));
#1563=EDGE_LOOP('',(#3443,#3444,#3445,#3446));
#1564=EDGE_LOOP('',(#3447,#3448,#3449,#3450));
#1565=EDGE_LOOP('',(#3451,#3452,#3453,#3454));
#1566=EDGE_LOOP('',(#3455,#3456,#3457,#3458));
#1567=EDGE_LOOP('',(#3459,#3460,#3461,#3462));
#1568=EDGE_LOOP('',(#3463,#3464,#3465,#3466));
#1569=EDGE_LOOP('',(#3467,#3468,#3469,#3470));
#1570=EDGE_LOOP('',(#3471,#3472,#3473,#3474));
#1571=EDGE_LOOP('',(#3475,#3476,#3477,#3478));
#1572=EDGE_LOOP('',(#3479,#3480,#3481,#3482));
#1573=EDGE_LOOP('',(#3483,#3484,#3485,#3486));
#1574=EDGE_LOOP('',(#3487,#3488,#3489,#3490));
#1575=EDGE_LOOP('',(#3491,#3492,#3493,#3494,#3495,#3496,#3497,#3498));
#1576=EDGE_LOOP('',(#3499));
#1577=EDGE_LOOP('',(#3500));
#1578=EDGE_LOOP('',(#3501));
#1579=EDGE_LOOP('',(#3502));
#1580=EDGE_LOOP('',(#3503));
#1581=EDGE_LOOP('',(#3504));
#1582=EDGE_LOOP('',(#3505));
#1583=EDGE_LOOP('',(#3506));
#1584=EDGE_LOOP('',(#3507,#3508,#3509,#3510,#3511,#3512,#3513,#3514));
#1585=EDGE_LOOP('',(#3515,#3516,#3517,#3518,#3519,#3520,#3521,#3522,#3523,
#3524,#3525,#3526));
#1586=EDGE_LOOP('',(#3527));
#1587=EDGE_LOOP('',(#3528));
#1588=EDGE_LOOP('',(#3529));
#1589=EDGE_LOOP('',(#3530,#3531,#3532,#3533));
#1590=EDGE_LOOP('',(#3534,#3535,#3536,#3537));
#1591=EDGE_LOOP('',(#3538,#3539,#3540,#3541));
#1592=EDGE_LOOP('',(#3542,#3543,#3544,#3545));
#1593=EDGE_LOOP('',(#3546));
#1594=EDGE_LOOP('',(#3547));
#1595=EDGE_LOOP('',(#3548,#3549,#3550,#3551));
#1596=EDGE_LOOP('',(#3552,#3553,#3554,#3555));
#1597=EDGE_LOOP('',(#3556));
#1598=EDGE_LOOP('',(#3557));
#1599=EDGE_LOOP('',(#3558,#3559,#3560,#3561));
#1600=EDGE_LOOP('',(#3562,#3563,#3564,#3565));
#1601=EDGE_LOOP('',(#3566));
#1602=EDGE_LOOP('',(#3567,#3568,#3569,#3570));
#1603=EDGE_LOOP('',(#3571));
#1604=EDGE_LOOP('',(#3572,#3573,#3574,#3575));
#1605=EDGE_LOOP('',(#3576,#3577,#3578,#3579));
#1606=EDGE_LOOP('',(#3580));
#1607=EDGE_LOOP('',(#3581));
#1608=EDGE_LOOP('',(#3582));
#1609=EDGE_LOOP('',(#3583));
#1610=EDGE_LOOP('',(#3584,#3585,#3586,#3587));
#1611=EDGE_LOOP('',(#3588));
#1612=EDGE_LOOP('',(#3589));
#1613=EDGE_LOOP('',(#3590));
#1614=EDGE_LOOP('',(#3591,#3592,#3593,#3594));
#1615=EDGE_LOOP('',(#3595));
#1616=EDGE_LOOP('',(#3596,#3597,#3598,#3599));
#1617=EDGE_LOOP('',(#3600));
#1618=EDGE_LOOP('',(#3601));
#1619=EDGE_LOOP('',(#3602,#3603,#3604,#3605));
#1620=EDGE_LOOP('',(#3606,#3607,#3608,#3609));
#1621=EDGE_LOOP('',(#3610));
#1622=EDGE_LOOP('',(#3611));
#1623=EDGE_LOOP('',(#3612));
#1624=EDGE_LOOP('',(#3613));
#1625=EDGE_LOOP('',(#3614,#3615,#3616,#3617));
#1626=EDGE_LOOP('',(#3618,#3619,#3620,#3621));
#1627=EDGE_LOOP('',(#3622));
#1628=EDGE_LOOP('',(#3623));
#1629=EDGE_LOOP('',(#3624));
#1630=EDGE_LOOP('',(#3625));
#1631=EDGE_LOOP('',(#3626,#3627,#3628,#3629));
#1632=EDGE_LOOP('',(#3630,#3631,#3632,#3633));
#1633=EDGE_LOOP('',(#3634));
#1634=EDGE_LOOP('',(#3635));
#1635=EDGE_LOOP('',(#3636));
#1636=EDGE_LOOP('',(#3637));
#1637=EDGE_LOOP('',(#3638,#3639,#3640,#3641));
#1638=EDGE_LOOP('',(#3642,#3643,#3644,#3645));
#1639=EDGE_LOOP('',(#3646));
#1640=EDGE_LOOP('',(#3647));
#1641=EDGE_LOOP('',(#3648));
#1642=EDGE_LOOP('',(#3649));
#1643=EDGE_LOOP('',(#3650,#3651,#3652,#3653));
#1644=EDGE_LOOP('',(#3654,#3655,#3656,#3657));
#1645=EDGE_LOOP('',(#3658));
#1646=EDGE_LOOP('',(#3659));
#1647=EDGE_LOOP('',(#3660));
#1648=EDGE_LOOP('',(#3661));
#1649=EDGE_LOOP('',(#3662,#3663,#3664,#3665));
#1650=EDGE_LOOP('',(#3666,#3667,#3668,#3669));
#1651=EDGE_LOOP('',(#3670));
#1652=EDGE_LOOP('',(#3671));
#1653=EDGE_LOOP('',(#3672));
#1654=EDGE_LOOP('',(#3673));
#1655=EDGE_LOOP('',(#3674,#3675,#3676,#3677));
#1656=EDGE_LOOP('',(#3678,#3679,#3680,#3681));
#1657=EDGE_LOOP('',(#3682));
#1658=EDGE_LOOP('',(#3683));
#1659=EDGE_LOOP('',(#3684));
#1660=EDGE_LOOP('',(#3685));
#1661=EDGE_LOOP('',(#3686,#3687,#3688,#3689));
#1662=EDGE_LOOP('',(#3690,#3691,#3692,#3693));
#1663=EDGE_LOOP('',(#3694,#3695,#3696,#3697));
#1664=EDGE_LOOP('',(#3698,#3699,#3700,#3701));
#1665=EDGE_LOOP('',(#3702,#3703,#3704,#3705));
#1666=EDGE_LOOP('',(#3706,#3707,#3708,#3709));
#1667=EDGE_LOOP('',(#3710,#3711,#3712,#3713,#3714,#3715));
#1668=EDGE_LOOP('',(#3716,#3717,#3718,#3719,#3720,#3721));
#1669=EDGE_LOOP('',(#3722));
#1670=EDGE_LOOP('',(#3723));
#1671=EDGE_LOOP('',(#3724,#3725,#3726,#3727));
#1672=EDGE_LOOP('',(#3728));
#1673=EDGE_LOOP('',(#3729));
#1674=EDGE_LOOP('',(#3730,#3731,#3732,#3733));
#1675=EDGE_LOOP('',(#3734,#3735,#3736,#3737));
#1676=EDGE_LOOP('',(#3738,#3739,#3740,#3741));
#1677=EDGE_LOOP('',(#3742));
#1678=EDGE_LOOP('',(#3743));
#1679=EDGE_LOOP('',(#3744,#3745,#3746,#3747));
#1680=EDGE_LOOP('',(#3748,#3749,#3750,#3751));
#1681=EDGE_LOOP('',(#3752,#3753,#3754,#3755));
#1682=EDGE_LOOP('',(#3756,#3757,#3758,#3759));
#1683=EDGE_LOOP('',(#3760));
#1684=EDGE_LOOP('',(#3761));
#1685=EDGE_LOOP('',(#3762));
#1686=EDGE_LOOP('',(#3763));
#1687=EDGE_LOOP('',(#3764,#3765,#3766,#3767,#3768,#3769,#3770,#3771,#3772));
#1688=EDGE_LOOP('',(#3773,#3774,#3775,#3776,#3777,#3778,#3779,#3780,#3781));
#1689=EDGE_LOOP('',(#3782,#3783,#3784,#3785));
#1690=EDGE_LOOP('',(#3786,#3787,#3788,#3789));
#1691=EDGE_LOOP('',(#3790,#3791,#3792,#3793));
#1692=EDGE_LOOP('',(#3794,#3795,#3796,#3797));
#1693=EDGE_LOOP('',(#3798,#3799,#3800,#3801));
#1694=EDGE_LOOP('',(#3802,#3803,#3804,#3805));
#1695=EDGE_LOOP('',(#3806,#3807,#3808,#3809));
#1696=EDGE_LOOP('',(#3810));
#1697=EDGE_LOOP('',(#3811));
#1698=EDGE_LOOP('',(#3812));
#1699=EDGE_LOOP('',(#3813));
#1700=EDGE_LOOP('',(#3814));
#1701=EDGE_LOOP('',(#3815,#3816,#3817,#3818));
#1702=EDGE_LOOP('',(#3819,#3820,#3821,#3822));
#1703=EDGE_LOOP('',(#3823,#3824,#3825,#3826));
#1704=EDGE_LOOP('',(#3827));
#1705=EDGE_LOOP('',(#3828));
#1706=EDGE_LOOP('',(#3829,#3830,#3831,#3832));
#1707=EDGE_LOOP('',(#3833,#3834,#3835,#3836));
#1708=EDGE_LOOP('',(#3837,#3838,#3839,#3840));
#1709=EDGE_LOOP('',(#3841));
#1710=EDGE_LOOP('',(#3842,#3843,#3844,#3845));
#1711=EDGE_LOOP('',(#3846,#3847,#3848,#3849));
#1712=EDGE_LOOP('',(#3850,#3851,#3852,#3853));
#1713=EDGE_LOOP('',(#3854,#3855,#3856,#3857));
#1714=EDGE_LOOP('',(#3858,#3859,#3860,#3861));
#1715=EDGE_LOOP('',(#3862,#3863,#3864,#3865));
#1716=EDGE_LOOP('',(#3866,#3867,#3868,#3869,#3870,#3871));
#1717=EDGE_LOOP('',(#3872,#3873,#3874,#3875,#3876,#3877));
#1718=EDGE_LOOP('',(#3878,#3879,#3880,#3881));
#1719=EDGE_LOOP('',(#3882,#3883,#3884,#3885));
#1720=EDGE_LOOP('',(#3886,#3887,#3888,#3889));
#1721=EDGE_LOOP('',(#3890,#3891,#3892,#3893));
#1722=EDGE_LOOP('',(#3894,#3895,#3896,#3897));
#1723=EDGE_LOOP('',(#3898,#3899,#3900,#3901));
#1724=EDGE_LOOP('',(#3902,#3903,#3904,#3905));
#1725=EDGE_LOOP('',(#3906));
#1726=EDGE_LOOP('',(#3907));
#1727=EDGE_LOOP('',(#3908));
#1728=EDGE_LOOP('',(#3909));
#1729=EDGE_LOOP('',(#3910,#3911,#3912,#3913));
#1730=EDGE_LOOP('',(#3914,#3915,#3916,#3917));
#1731=EDGE_LOOP('',(#3918,#3919,#3920,#3921));
#1732=EDGE_LOOP('',(#3922,#3923,#3924,#3925));
#1733=EDGE_LOOP('',(#3926));
#1734=EDGE_LOOP('',(#3927));
#1735=EDGE_LOOP('',(#3928));
#1736=EDGE_LOOP('',(#3929));
#1737=EDGE_LOOP('',(#3930));
#1738=EDGE_LOOP('',(#3931));
#1739=EDGE_LOOP('',(#3932));
#1740=EDGE_LOOP('',(#3933));
#1741=EDGE_LOOP('',(#3934));
#1742=EDGE_LOOP('',(#3935));
#1743=EDGE_LOOP('',(#3936));
#1744=EDGE_LOOP('',(#3937));
#1745=EDGE_LOOP('',(#3938,#3939,#3940,#3941));
#1746=EDGE_LOOP('',(#3942,#3943,#3944,#3945));
#1747=EDGE_LOOP('',(#3946));
#1748=EDGE_LOOP('',(#3947));
#1749=EDGE_LOOP('',(#3948));
#1750=EDGE_LOOP('',(#3949));
#1751=EDGE_LOOP('',(#3950,#3951,#3952,#3953));
#1752=EDGE_LOOP('',(#3954,#3955,#3956,#3957));
#1753=EDGE_LOOP('',(#3958,#3959,#3960,#3961));
#1754=EDGE_LOOP('',(#3962,#3963,#3964,#3965));
#1755=EDGE_LOOP('',(#3966,#3967,#3968,#3969));
#1756=EDGE_LOOP('',(#3970));
#1757=EDGE_LOOP('',(#3971));
#1758=EDGE_LOOP('',(#3972,#3973,#3974,#3975));
#1759=EDGE_LOOP('',(#3976,#3977,#3978,#3979));
#1760=EDGE_LOOP('',(#3980));
#1761=EDGE_LOOP('',(#3981));
#1762=EDGE_LOOP('',(#3982));
#1763=EDGE_LOOP('',(#3983));
#1764=EDGE_LOOP('',(#3984));
#1765=EDGE_LOOP('',(#3985));
#1766=EDGE_LOOP('',(#3986));
#1767=EDGE_LOOP('',(#3987));
#1768=EDGE_LOOP('',(#3988));
#1769=EDGE_LOOP('',(#3989));
#1770=EDGE_LOOP('',(#3990));
#1771=EDGE_LOOP('',(#3991));
#1772=EDGE_LOOP('',(#3992,#3993,#3994,#3995));
#1773=EDGE_LOOP('',(#3996,#3997,#3998,#3999));
#1774=EDGE_LOOP('',(#4000,#4001,#4002,#4003));
#1775=EDGE_LOOP('',(#4004,#4005,#4006,#4007));
#1776=EDGE_LOOP('',(#4008,#4009,#4010,#4011));
#1777=EDGE_LOOP('',(#4012));
#1778=EDGE_LOOP('',(#4013));
#1779=EDGE_LOOP('',(#4014,#4015,#4016,#4017));
#1780=EDGE_LOOP('',(#4018,#4019,#4020,#4021));
#1781=EDGE_LOOP('',(#4022));
#1782=EDGE_LOOP('',(#4023));
#1783=EDGE_LOOP('',(#4024));
#1784=EDGE_LOOP('',(#4025));
#1785=EDGE_LOOP('',(#4026));
#1786=EDGE_LOOP('',(#4027));
#1787=EDGE_LOOP('',(#4028));
#1788=EDGE_LOOP('',(#4029));
#1789=EDGE_LOOP('',(#4030));
#1790=EDGE_LOOP('',(#4031));
#1791=EDGE_LOOP('',(#4032));
#1792=EDGE_LOOP('',(#4033));
#1793=EDGE_LOOP('',(#4034,#4035,#4036,#4037,#4038,#4039));
#1794=EDGE_LOOP('',(#4040,#4041,#4042,#4043,#4044));
#1795=EDGE_LOOP('',(#4045,#4046,#4047,#4048));
#1796=EDGE_LOOP('',(#4049,#4050,#4051,#4052));
#1797=EDGE_LOOP('',(#4053));
#1798=EDGE_LOOP('',(#4054));
#1799=EDGE_LOOP('',(#4055,#4056,#4057,#4058,#4059));
#1800=EDGE_LOOP('',(#4060));
#1801=EDGE_LOOP('',(#4061));
#1802=EDGE_LOOP('',(#4062,#4063,#4064,#4065));
#1803=EDGE_LOOP('',(#4066,#4067,#4068,#4069,#4070,#4071));
#1804=EDGE_LOOP('',(#4072,#4073,#4074,#4075,#4076));
#1805=EDGE_LOOP('',(#4077));
#1806=EDGE_LOOP('',(#4078));
#1807=EDGE_LOOP('',(#4079,#4080,#4081,#4082));
#1808=EDGE_LOOP('',(#4083,#4084,#4085,#4086));
#1809=EDGE_LOOP('',(#4087,#4088,#4089,#4090));
#1810=EDGE_LOOP('',(#4091));
#1811=EDGE_LOOP('',(#4092));
#1812=EDGE_LOOP('',(#4093,#4094,#4095,#4096,#4097));
#1813=EDGE_LOOP('',(#4098,#4099));
#1814=EDGE_LOOP('',(#4100,#4101));
#1815=EDGE_LOOP('',(#4102,#4103));
#1816=EDGE_LOOP('',(#4104,#4105));
#1817=EDGE_LOOP('',(#4106,#4107));
#1818=EDGE_LOOP('',(#4108,#4109));
#1819=EDGE_LOOP('',(#4110,#4111));
#1820=EDGE_LOOP('',(#4112,#4113));
#1821=EDGE_LOOP('',(#4114,#4115,#4116,#4117));
#1822=EDGE_LOOP('',(#4118,#4119,#4120,#4121,#4122,#4123,#4124,#4125,#4126,
#4127,#4128,#4129,#4130,#4131,#4132,#4133,#4134,#4135,#4136,#4137));
#1823=EDGE_LOOP('',(#4138,#4139,#4140,#4141));
#1824=EDGE_LOOP('',(#4142,#4143,#4144,#4145));
#1825=EDGE_LOOP('',(#4146,#4147,#4148,#4149));
#1826=EDGE_LOOP('',(#4150,#4151,#4152,#4153));
#1827=EDGE_LOOP('',(#4154,#4155,#4156,#4157));
#1828=EDGE_LOOP('',(#4158,#4159,#4160,#4161,#4162,#4163));
#1829=EDGE_LOOP('',(#4164,#4165,#4166,#4167));
#1830=EDGE_LOOP('',(#4168,#4169,#4170,#4171));
#1831=EDGE_LOOP('',(#4172,#4173,#4174,#4175));
#1832=EDGE_LOOP('',(#4176,#4177,#4178,#4179));
#1833=EDGE_LOOP('',(#4180,#4181,#4182,#4183));
#1834=EDGE_LOOP('',(#4184,#4185,#4186,#4187));
#1835=EDGE_LOOP('',(#4188,#4189,#4190,#4191,#4192,#4193,#4194,#4195,#4196,
#4197,#4198,#4199,#4200,#4201,#4202,#4203,#4204,#4205,#4206,#4207));
#1836=EDGE_LOOP('',(#4208,#4209,#4210,#4211));
#1837=EDGE_LOOP('',(#4212,#4213,#4214,#4215));
#1838=EDGE_LOOP('',(#4216));
#1839=EDGE_LOOP('',(#4217));
#1840=EDGE_LOOP('',(#4218,#4219,#4220,#4221));
#1841=EDGE_LOOP('',(#4222));
#1842=EDGE_LOOP('',(#4223));
#1843=EDGE_LOOP('',(#4224,#4225,#4226,#4227));
#1844=EDGE_LOOP('',(#4228));
#1845=EDGE_LOOP('',(#4229));
#1846=EDGE_LOOP('',(#4230,#4231,#4232,#4233));
#1847=EDGE_LOOP('',(#4234));
#1848=EDGE_LOOP('',(#4235));
#1849=EDGE_LOOP('',(#4236,#4237,#4238,#4239));
#1850=EDGE_LOOP('',(#4240));
#1851=EDGE_LOOP('',(#4241));
#1852=EDGE_LOOP('',(#4242,#4243,#4244,#4245));
#1853=EDGE_LOOP('',(#4246,#4247,#4248,#4249));
#1854=EDGE_LOOP('',(#4250,#4251,#4252,#4253));
#1855=EDGE_LOOP('',(#4254,#4255,#4256,#4257));
#1856=EDGE_LOOP('',(#4258,#4259,#4260,#4261));
#1857=EDGE_LOOP('',(#4262,#4263,#4264,#4265));
#1858=EDGE_LOOP('',(#4266,#4267,#4268,#4269));
#1859=EDGE_LOOP('',(#4270,#4271,#4272,#4273,#4274,#4275));
#1860=EDGE_LOOP('',(#4276,#4277,#4278,#4279,#4280,#4281));
#1861=EDGE_LOOP('',(#4282));
#1862=EDGE_LOOP('',(#4283));
#1863=EDGE_LOOP('',(#4284,#4285,#4286,#4287));
#1864=EDGE_LOOP('',(#4288,#4289,#4290,#4291));
#1865=EDGE_LOOP('',(#4292,#4293,#4294,#4295));
#1866=EDGE_LOOP('',(#4296));
#1867=EDGE_LOOP('',(#4297));
#1868=EDGE_LOOP('',(#4298,#4299,#4300,#4301));
#1869=EDGE_LOOP('',(#4302,#4303,#4304,#4305));
#1870=EDGE_LOOP('',(#4306));
#1871=EDGE_LOOP('',(#4307));
#1872=EDGE_LOOP('',(#4308));
#1873=EDGE_LOOP('',(#4309));
#1874=EDGE_LOOP('',(#4310,#4311,#4312,#4313));
#1875=EDGE_LOOP('',(#4314,#4315,#4316,#4317,#4318,#4319));
#1876=EDGE_LOOP('',(#4320,#4321,#4322,#4323));
#1877=EDGE_LOOP('',(#4324));
#1878=EDGE_LOOP('',(#4325,#4326,#4327,#4328));
#1879=EDGE_LOOP('',(#4329,#4330,#4331,#4332,#4333));
#1880=EDGE_LOOP('',(#4334,#4335,#4336,#4337));
#1881=EDGE_LOOP('',(#4338,#4339,#4340,#4341));
#1882=EDGE_LOOP('',(#4342,#4343,#4344,#4345,#4346,#4347,#4348,#4349));
#1883=EDGE_LOOP('',(#4350,#4351,#4352,#4353));
#1884=EDGE_LOOP('',(#4354,#4355,#4356,#4357,#4358,#4359,#4360,#4361));
#1885=EDGE_LOOP('',(#4362,#4363,#4364,#4365));
#1886=EDGE_LOOP('',(#4366,#4367,#4368,#4369));
#1887=EDGE_LOOP('',(#4370,#4371,#4372,#4373));
#1888=EDGE_LOOP('',(#4374,#4375,#4376,#4377));
#1889=EDGE_LOOP('',(#4378,#4379,#4380,#4381));
#1890=EDGE_LOOP('',(#4382));
#1891=EDGE_LOOP('',(#4383));
#1892=EDGE_LOOP('',(#4384));
#1893=EDGE_LOOP('',(#4385));
#1894=EDGE_LOOP('',(#4386,#4387,#4388,#4389));
#1895=EDGE_LOOP('',(#4390,#4391,#4392,#4393));
#1896=EDGE_LOOP('',(#4394,#4395,#4396,#4397));
#1897=EDGE_LOOP('',(#4398,#4399,#4400,#4401));
#1898=EDGE_LOOP('',(#4402,#4403,#4404,#4405));
#1899=EDGE_LOOP('',(#4406,#4407,#4408,#4409));
#1900=EDGE_LOOP('',(#4410,#4411,#4412,#4413));
#1901=EDGE_LOOP('',(#4414,#4415,#4416,#4417,#4418,#4419));
#1902=EDGE_LOOP('',(#4420));
#1903=EDGE_LOOP('',(#4421,#4422,#4423,#4424,#4425,#4426));
#1904=EDGE_LOOP('',(#4427));
#1905=EDGE_LOOP('',(#4428,#4429,#4430,#4431));
#1906=EDGE_LOOP('',(#4432,#4433,#4434,#4435));
#1907=EDGE_LOOP('',(#4436,#4437,#4438,#4439));
#1908=EDGE_LOOP('',(#4440,#4441));
#1909=EDGE_LOOP('',(#4442));
#1910=EDGE_LOOP('',(#4443));
#1911=EDGE_LOOP('',(#4444,#4445,#4446,#4447));
#1912=EDGE_LOOP('',(#4448,#4449));
#1913=EDGE_LOOP('',(#4450));
#1914=EDGE_LOOP('',(#4451));
#1915=CIRCLE('',#5263,0.9);
#1916=CIRCLE('',#5264,3.25);
#1917=CIRCLE('',#5265,0.9);
#1918=CIRCLE('',#5266,3.25);
#1919=CIRCLE('',#5267,0.9);
#1920=CIRCLE('',#5268,3.25);
#1921=CIRCLE('',#5269,0.9);
#1922=CIRCLE('',#5270,3.25);
#1923=CIRCLE('',#5271,1.2);
#1924=CIRCLE('',#5273,3.25);
#1925=CIRCLE('',#5275,3.25);
#1926=CIRCLE('',#5277,3.25);
#1927=CIRCLE('',#5279,1.2);
#1928=CIRCLE('',#5281,3.25);
#1929=CIRCLE('',#5283,0.9);
#1930=CIRCLE('',#5284,0.9);
#1931=CIRCLE('',#5285,0.9);
#1932=CIRCLE('',#5287,0.9);
#1933=CIRCLE('',#5288,0.9);
#1934=CIRCLE('',#5289,0.9);
#1935=CIRCLE('',#5291,0.9);
#1936=CIRCLE('',#5292,0.9);
#1937=CIRCLE('',#5293,0.9);
#1938=CIRCLE('',#5295,1.);
#1939=CIRCLE('',#5297,0.9);
#1940=CIRCLE('',#5298,0.9);
#1941=CIRCLE('',#5299,0.9);
#1942=CIRCLE('',#5301,0.425);
#1943=CIRCLE('',#5302,0.425);
#1944=CIRCLE('',#5304,0.425);
#1945=CIRCLE('',#5305,0.425);
#1946=CIRCLE('',#5307,0.425);
#1947=CIRCLE('',#5308,0.425);
#1948=CIRCLE('',#5310,1.);
#1949=CIRCLE('',#5323,0.9);
#1950=CIRCLE('',#5324,3.25);
#1951=CIRCLE('',#5325,0.9);
#1952=CIRCLE('',#5326,3.25);
#1953=CIRCLE('',#5327,0.9);
#1954=CIRCLE('',#5328,3.25);
#1955=CIRCLE('',#5329,0.9);
#1956=CIRCLE('',#5330,3.25);
#1957=CIRCLE('',#5331,1.2);
#1958=CIRCLE('',#5333,3.25);
#1959=CIRCLE('',#5335,3.25);
#1960=CIRCLE('',#5337,3.25);
#1961=CIRCLE('',#5339,1.2);
#1962=CIRCLE('',#5341,3.25);
#1963=CIRCLE('',#5343,0.9);
#1964=CIRCLE('',#5344,0.9);
#1965=CIRCLE('',#5345,0.9);
#1966=CIRCLE('',#5347,0.9);
#1967=CIRCLE('',#5348,0.9);
#1968=CIRCLE('',#5349,0.9);
#1969=CIRCLE('',#5351,1.);
#1970=CIRCLE('',#5353,0.9);
#1971=CIRCLE('',#5354,0.9);
#1972=CIRCLE('',#5355,0.9);
#1973=CIRCLE('',#5357,0.9);
#1974=CIRCLE('',#5358,0.9);
#1975=CIRCLE('',#5359,0.9);
#1976=CIRCLE('',#5361,0.425);
#1977=CIRCLE('',#5362,0.425);
#1978=CIRCLE('',#5364,0.425);
#1979=CIRCLE('',#5365,0.425);
#1980=CIRCLE('',#5367,0.425);
#1981=CIRCLE('',#5368,0.425);
#1982=CIRCLE('',#5370,1.);
#1983=CIRCLE('',#5383,1.1);
#1984=CIRCLE('',#5384,1.1);
#1985=CIRCLE('',#5386,0.425);
#1986=CIRCLE('',#5387,0.425);
#1987=CIRCLE('',#5389,0.425);
#1988=CIRCLE('',#5390,0.425);
#1989=CIRCLE('',#5399,0.425);
#1990=CIRCLE('',#5400,0.425);
#1991=CIRCLE('',#5402,1.);
#1992=CIRCLE('',#5403,1.);
#1993=CIRCLE('',#5408,0.34);
#1994=CIRCLE('',#5409,0.34);
#1995=CIRCLE('',#5412,1.5);
#1996=CIRCLE('',#5413,1.);
#1997=CIRCLE('',#5415,1.5);
#1998=CIRCLE('',#5418,1.);
#1999=CIRCLE('',#5422,0.425);
#2000=CIRCLE('',#5423,0.425);
#2001=CIRCLE('',#5425,1.5);
#2002=CIRCLE('',#5426,1.5);
#2003=CIRCLE('',#5431,1.005);
#2004=CIRCLE('',#5432,1.005);
#2005=CIRCLE('',#5434,1.4);
#2006=CIRCLE('',#5435,1.4);
#2007=CIRCLE('',#5440,1.005);
#2008=CIRCLE('',#5441,1.005);
#2009=CIRCLE('',#5443,1.4);
#2010=CIRCLE('',#5444,1.4);
#2011=CIRCLE('',#5449,1.005);
#2012=CIRCLE('',#5450,1.005);
#2013=CIRCLE('',#5452,1.4);
#2014=CIRCLE('',#5453,1.4);
#2015=CIRCLE('',#5458,0.81);
#2016=CIRCLE('',#5459,0.81);
#2017=CIRCLE('',#5461,1.1);
#2018=CIRCLE('',#5462,1.1);
#2019=CIRCLE('',#5467,1.005);
#2020=CIRCLE('',#5468,1.005);
#2021=CIRCLE('',#5470,1.4);
#2022=CIRCLE('',#5471,1.4);
#2023=CIRCLE('',#5476,1.005);
#2024=CIRCLE('',#5477,1.005);
#2025=CIRCLE('',#5479,1.4);
#2026=CIRCLE('',#5480,1.4);
#2027=CIRCLE('',#5493,0.4);
#2028=CIRCLE('',#5494,0.3933);
#2029=CIRCLE('',#5496,0.4);
#2030=CIRCLE('',#5499,0.6);
#2031=CIRCLE('',#5501,0.65);
#2032=CIRCLE('',#5503,0.65);
#2033=CIRCLE('',#5505,0.62);
#2034=CIRCLE('',#5507,0.42);
#2035=CIRCLE('',#5509,0.3933);
#2036=CIRCLE('',#5513,0.42);
#2037=CIRCLE('',#5514,0.42);
#2038=CIRCLE('',#5516,0.8);
#2039=CIRCLE('',#5517,0.8);
#2040=CIRCLE('',#5522,0.6175);
#2041=CIRCLE('',#5524,0.6175);
#2042=CIRCLE('',#5529,0.338975);
#2043=CIRCLE('',#5530,0.338975);
#2044=CIRCLE('',#5538,0.6);
#2045=CIRCLE('',#5540,0.65);
#2046=CIRCLE('',#5542,0.65);
#2047=CIRCLE('',#5544,0.62);
#2048=CIRCLE('',#5546,0.42);
#2049=CIRCLE('',#5548,0.3933);
#2050=CIRCLE('',#5550,0.3933);
#2051=CIRCLE('',#5552,0.32);
#2052=CIRCLE('',#5590,0.165);
#2053=CIRCLE('',#5591,0.165);
#2054=CIRCLE('',#5593,0.165);
#2055=CIRCLE('',#5594,0.165);
#2056=CIRCLE('',#5596,0.165);
#2057=CIRCLE('',#5597,0.165);
#2058=CIRCLE('',#5599,0.165);
#2059=CIRCLE('',#5600,0.165);
#2060=CIRCLE('',#5602,4.4);
#2061=CIRCLE('',#5603,5.);
#2062=CIRCLE('',#5605,5.);
#2063=CIRCLE('',#5607,5.);
#2064=CIRCLE('',#5609,3.);
#2065=CIRCLE('',#5611,5.);
#2066=CIRCLE('',#5612,3.);
#2067=CIRCLE('',#5615,3.);
#2068=CIRCLE('',#5617,2.35);
#2069=CIRCLE('',#5618,2.35);
#2070=CIRCLE('',#5620,3.);
#2071=CIRCLE('',#5625,1.9);
#2072=CIRCLE('',#5626,1.9);
#2073=CIRCLE('',#5628,2.34);
#2074=CIRCLE('',#5629,2.34);
#2075=CIRCLE('',#5634,0.225);
#2076=CIRCLE('',#5635,0.225);
#2077=CIRCLE('',#5637,0.225);
#2078=CIRCLE('',#5638,0.225);
#2079=CIRCLE('',#5640,0.225);
#2080=CIRCLE('',#5641,0.225);
#2081=CIRCLE('',#5643,0.225);
#2082=CIRCLE('',#5644,0.225);
#2083=CIRCLE('',#5646,2.34);
#2084=CIRCLE('',#5647,2.34);
#2085=CIRCLE('',#5649,1.9);
#2086=CIRCLE('',#5651,1.9);
#2087=CIRCLE('',#5653,3.);
#2088=CIRCLE('',#5654,3.);
#2089=CIRCLE('',#5659,0.225);
#2090=CIRCLE('',#5660,0.225);
#2091=CIRCLE('',#5662,0.225);
#2092=CIRCLE('',#5663,0.225);
#2093=CIRCLE('',#5665,0.225);
#2094=CIRCLE('',#5666,0.225);
#2095=CIRCLE('',#5668,0.225);
#2096=CIRCLE('',#5669,0.225);
#2097=CIRCLE('',#5671,2.34);
#2098=CIRCLE('',#5672,2.34);
#2099=CIRCLE('',#5674,1.9);
#2100=CIRCLE('',#5676,1.9);
#2101=CIRCLE('',#5678,3.);
#2102=CIRCLE('',#5679,3.);
#2103=CIRCLE('',#5685,1.63531);
#2104=CIRCLE('',#5686,1.63531);
#2105=CIRCLE('',#5687,0.412776);
#2106=CIRCLE('',#5688,1.63531);
#2107=CIRCLE('',#5689,1.63531);
#2108=CIRCLE('',#5691,1.63531);
#2109=CIRCLE('',#5693,1.);
#2110=CIRCLE('',#5694,1.);
#2111=CIRCLE('',#5696,1.1);
#2112=CIRCLE('',#5699,1.63531);
#2113=CIRCLE('',#5701,1.1);
#2114=CIRCLE('',#5705,1.71469);
#2115=CIRCLE('',#5706,1.71469);
#2116=CIRCLE('',#5707,0.412776);
#2117=CIRCLE('',#5708,1.71469);
#2118=CIRCLE('',#5709,1.71469);
#2119=CIRCLE('',#5711,1.71469);
#2120=CIRCLE('',#5713,2.25);
#2121=CIRCLE('',#5714,1.71469);
#2122=CIRCLE('',#5716,2.35);
#2123=CIRCLE('',#5718,2.35);
#2124=CIRCLE('',#5720,2.25);
#2125=CIRCLE('',#5725,0.3969);
#2126=CIRCLE('',#5727,0.3969);
#2127=CIRCLE('',#5729,0.3969);
#2128=CIRCLE('',#5731,0.3969);
#2129=CIRCLE('',#5733,0.3969);
#2130=CIRCLE('',#5735,0.3969);
#2131=CIRCLE('',#5737,0.3969);
#2132=CIRCLE('',#5739,0.3969);
#2133=CIRCLE('',#5742,0.405071403305639);
#2134=CIRCLE('',#5743,0.405071403305639);
#2135=CIRCLE('',#5745,1.706752);
#2136=CIRCLE('',#5746,1.706752);
#2137=CIRCLE('',#5747,1.706752);
#2138=CIRCLE('',#5748,1.706752);
#2139=CIRCLE('',#5749,1.706752);
#2140=CIRCLE('',#5750,1.706752);
#2141=CIRCLE('',#5751,1.706752);
#2142=CIRCLE('',#5752,1.706752);
#2143=CIRCLE('',#5753,1.706752);
#2144=CIRCLE('',#5755,1.643248);
#2145=CIRCLE('',#5756,0.405071403305639);
#2146=CIRCLE('',#5758,0.405071403305639);
#2147=CIRCLE('',#5760,1.643248);
#2148=CIRCLE('',#5761,0.405071403305639);
#2149=CIRCLE('',#5763,0.405071403305639);
#2150=CIRCLE('',#5765,1.643248);
#2151=CIRCLE('',#5766,0.405071403305639);
#2152=CIRCLE('',#5768,0.405071403305639);
#2153=CIRCLE('',#5770,1.643248);
#2154=CIRCLE('',#5771,0.405071403305639);
#2155=CIRCLE('',#5773,0.405071403305639);
#2156=CIRCLE('',#5775,1.643248);
#2157=CIRCLE('',#5776,0.405071403305639);
#2158=CIRCLE('',#5778,0.405071403305639);
#2159=CIRCLE('',#5780,1.643248);
#2160=CIRCLE('',#5781,0.405071403305639);
#2161=CIRCLE('',#5783,0.405071403305639);
#2162=CIRCLE('',#5785,1.643248);
#2163=CIRCLE('',#5786,1.643248);
#2164=CIRCLE('',#5787,1.643248);
#2165=CIRCLE('',#5789,0.405071403305639);
#2166=CIRCLE('',#5791,0.405071403305639);
#2167=CIRCLE('',#5796,1.70469);
#2168=CIRCLE('',#5797,1.65031);
#2169=CIRCLE('',#5799,1.70469);
#2170=CIRCLE('',#5801,1.65031);
#2171=CIRCLE('',#5804,1.70469);
#2172=CIRCLE('',#5805,1.65031);
#2173=CIRCLE('',#5807,1.70469);
#2174=CIRCLE('',#5809,1.65031);
#2175=CIRCLE('',#5826,0.1954);
#2176=CIRCLE('',#5828,0.3);
#2177=CIRCLE('',#5830,0.35);
#2178=CIRCLE('',#5832,0.35);
#2179=CIRCLE('',#5834,0.32);
#2180=CIRCLE('',#5836,0.22);
#2181=CIRCLE('',#5838,0.1954);
#2182=CIRCLE('',#5857,1.3);
#2183=CIRCLE('',#5858,0.8);
#2184=CIRCLE('',#5860,1.3);
#2185=CIRCLE('',#5861,0.8);
#2186=CIRCLE('',#5864,0.8);
#2187=CIRCLE('',#5865,0.8);
#2188=CIRCLE('',#5866,0.8);
#2189=CIRCLE('',#5868,0.8);
#2190=CIRCLE('',#5875,2.);
#2191=CIRCLE('',#5876,3.5);
#2192=CIRCLE('',#5878,2.);
#2193=CIRCLE('',#5880,3.5);
#2194=CIRCLE('',#5886,0.81);
#2195=CIRCLE('',#5887,0.81);
#2196=CIRCLE('',#5889,1.5);
#2197=CIRCLE('',#5890,1.5);
#2198=CIRCLE('',#5895,0.7);
#2199=CIRCLE('',#5896,0.7);
#2200=CIRCLE('',#5911,1.);
#2201=CIRCLE('',#5912,1.);
#2202=CIRCLE('',#5914,1.);
#2203=CIRCLE('',#5915,1.);
#2204=CIRCLE('',#5917,2.);
#2205=CIRCLE('',#5918,2.);
#2206=CIRCLE('',#5920,2.);
#2207=CIRCLE('',#5922,2.);
#2208=VERTEX_POINT('',#7561);
#2209=VERTEX_POINT('',#7562);
#2210=VERTEX_POINT('',#7564);
#2211=VERTEX_POINT('',#7566);
#2212=VERTEX_POINT('',#7568);
#2213=VERTEX_POINT('',#7570);
#2214=VERTEX_POINT('',#7572);
#2215=VERTEX_POINT('',#7574);
#2216=VERTEX_POINT('',#7577);
#2217=VERTEX_POINT('',#7580);
#2218=VERTEX_POINT('',#7582);
#2219=VERTEX_POINT('',#7586);
#2220=VERTEX_POINT('',#7588);
#2221=VERTEX_POINT('',#7592);
#2222=VERTEX_POINT('',#7594);
#2223=VERTEX_POINT('',#7598);
#2224=VERTEX_POINT('',#7602);
#2225=VERTEX_POINT('',#7604);
#2226=VERTEX_POINT('',#7608);
#2227=VERTEX_POINT('',#7610);
#2228=VERTEX_POINT('',#7615);
#2229=VERTEX_POINT('',#7617);
#2230=VERTEX_POINT('',#7622);
#2231=VERTEX_POINT('',#7624);
#2232=VERTEX_POINT('',#7629);
#2233=VERTEX_POINT('',#7632);
#2234=VERTEX_POINT('',#7634);
#2235=VERTEX_POINT('',#7639);
#2236=VERTEX_POINT('',#7641);
#2237=VERTEX_POINT('',#7645);
#2238=VERTEX_POINT('',#7647);
#2239=VERTEX_POINT('',#7651);
#2240=VERTEX_POINT('',#7653);
#2241=VERTEX_POINT('',#7657);
#2242=VERTEX_POINT('',#7661);
#2243=VERTEX_POINT('',#7662);
#2244=VERTEX_POINT('',#7664);
#2245=VERTEX_POINT('',#7666);
#2246=VERTEX_POINT('',#7670);
#2247=VERTEX_POINT('',#7672);
#2248=VERTEX_POINT('',#7676);
#2249=VERTEX_POINT('',#7678);
#2250=VERTEX_POINT('',#7682);
#2251=VERTEX_POINT('',#7684);
#2252=VERTEX_POINT('',#7688);
#2253=VERTEX_POINT('',#7690);
#2254=VERTEX_POINT('',#7694);
#2255=VERTEX_POINT('',#7696);
#2256=VERTEX_POINT('',#7700);
#2257=VERTEX_POINT('',#7702);
#2258=VERTEX_POINT('',#7712);
#2259=VERTEX_POINT('',#7713);
#2260=VERTEX_POINT('',#7715);
#2261=VERTEX_POINT('',#7717);
#2262=VERTEX_POINT('',#7719);
#2263=VERTEX_POINT('',#7721);
#2264=VERTEX_POINT('',#7723);
#2265=VERTEX_POINT('',#7725);
#2266=VERTEX_POINT('',#7728);
#2267=VERTEX_POINT('',#7731);
#2268=VERTEX_POINT('',#7733);
#2269=VERTEX_POINT('',#7737);
#2270=VERTEX_POINT('',#7739);
#2271=VERTEX_POINT('',#7743);
#2272=VERTEX_POINT('',#7745);
#2273=VERTEX_POINT('',#7749);
#2274=VERTEX_POINT('',#7753);
#2275=VERTEX_POINT('',#7755);
#2276=VERTEX_POINT('',#7759);
#2277=VERTEX_POINT('',#7761);
#2278=VERTEX_POINT('',#7766);
#2279=VERTEX_POINT('',#7768);
#2280=VERTEX_POINT('',#7773);
#2281=VERTEX_POINT('',#7776);
#2282=VERTEX_POINT('',#7778);
#2283=VERTEX_POINT('',#7783);
#2284=VERTEX_POINT('',#7785);
#2285=VERTEX_POINT('',#7790);
#2286=VERTEX_POINT('',#7792);
#2287=VERTEX_POINT('',#7796);
#2288=VERTEX_POINT('',#7798);
#2289=VERTEX_POINT('',#7802);
#2290=VERTEX_POINT('',#7804);
#2291=VERTEX_POINT('',#7808);
#2292=VERTEX_POINT('',#7812);
#2293=VERTEX_POINT('',#7813);
#2294=VERTEX_POINT('',#7815);
#2295=VERTEX_POINT('',#7817);
#2296=VERTEX_POINT('',#7821);
#2297=VERTEX_POINT('',#7823);
#2298=VERTEX_POINT('',#7827);
#2299=VERTEX_POINT('',#7829);
#2300=VERTEX_POINT('',#7833);
#2301=VERTEX_POINT('',#7835);
#2302=VERTEX_POINT('',#7839);
#2303=VERTEX_POINT('',#7841);
#2304=VERTEX_POINT('',#7845);
#2305=VERTEX_POINT('',#7847);
#2306=VERTEX_POINT('',#7851);
#2307=VERTEX_POINT('',#7853);
#2308=VERTEX_POINT('',#7863);
#2309=VERTEX_POINT('',#7865);
#2310=VERTEX_POINT('',#7869);
#2311=VERTEX_POINT('',#7871);
#2312=VERTEX_POINT('',#7875);
#2313=VERTEX_POINT('',#7877);
#2314=VERTEX_POINT('',#7881);
#2315=VERTEX_POINT('',#7882);
#2316=VERTEX_POINT('',#7884);
#2317=VERTEX_POINT('',#7886);
#2318=VERTEX_POINT('',#7890);
#2319=VERTEX_POINT('',#7892);
#2320=VERTEX_POINT('',#7896);
#2321=VERTEX_POINT('',#7898);
#2322=VERTEX_POINT('',#7908);
#2323=VERTEX_POINT('',#7910);
#2324=VERTEX_POINT('',#7914);
#2325=VERTEX_POINT('',#7916);
#2326=VERTEX_POINT('',#7923);
#2327=VERTEX_POINT('',#7925);
#2328=VERTEX_POINT('',#7930);
#2329=VERTEX_POINT('',#7932);
#2330=VERTEX_POINT('',#7935);
#2331=VERTEX_POINT('',#7940);
#2332=VERTEX_POINT('',#7946);
#2333=VERTEX_POINT('',#7948);
#2334=VERTEX_POINT('',#7952);
#2335=VERTEX_POINT('',#7954);
#2336=VERTEX_POINT('',#7961);
#2337=VERTEX_POINT('',#7963);
#2338=VERTEX_POINT('',#7967);
#2339=VERTEX_POINT('',#7969);
#2340=VERTEX_POINT('',#7976);
#2341=VERTEX_POINT('',#7978);
#2342=VERTEX_POINT('',#7982);
#2343=VERTEX_POINT('',#7984);
#2344=VERTEX_POINT('',#7991);
#2345=VERTEX_POINT('',#7993);
#2346=VERTEX_POINT('',#7997);
#2347=VERTEX_POINT('',#7999);
#2348=VERTEX_POINT('',#8006);
#2349=VERTEX_POINT('',#8008);
#2350=VERTEX_POINT('',#8012);
#2351=VERTEX_POINT('',#8014);
#2352=VERTEX_POINT('',#8021);
#2353=VERTEX_POINT('',#8023);
#2354=VERTEX_POINT('',#8027);
#2355=VERTEX_POINT('',#8029);
#2356=VERTEX_POINT('',#8036);
#2357=VERTEX_POINT('',#8038);
#2358=VERTEX_POINT('',#8042);
#2359=VERTEX_POINT('',#8044);
#2360=VERTEX_POINT('',#8051);
#2361=VERTEX_POINT('',#8052);
#2362=VERTEX_POINT('',#8054);
#2363=VERTEX_POINT('',#8056);
#2364=VERTEX_POINT('',#8060);
#2365=VERTEX_POINT('',#8062);
#2366=VERTEX_POINT('',#8066);
#2367=VERTEX_POINT('',#8068);
#2368=VERTEX_POINT('',#8072);
#2369=VERTEX_POINT('',#8074);
#2370=VERTEX_POINT('',#8078);
#2371=VERTEX_POINT('',#8080);
#2372=VERTEX_POINT('',#8089);
#2373=VERTEX_POINT('',#8091);
#2374=VERTEX_POINT('',#8094);
#2375=VERTEX_POINT('',#8099);
#2376=VERTEX_POINT('',#8102);
#2377=VERTEX_POINT('',#8106);
#2378=VERTEX_POINT('',#8110);
#2379=VERTEX_POINT('',#8114);
#2380=VERTEX_POINT('',#8117);
#2381=VERTEX_POINT('',#8124);
#2382=VERTEX_POINT('',#8126);
#2383=VERTEX_POINT('',#8130);
#2384=VERTEX_POINT('',#8132);
#2385=VERTEX_POINT('',#8139);
#2386=VERTEX_POINT('',#8140);
#2387=VERTEX_POINT('',#8144);
#2388=VERTEX_POINT('',#8148);
#2389=VERTEX_POINT('',#8151);
#2390=VERTEX_POINT('',#8155);
#2391=VERTEX_POINT('',#8159);
#2392=VERTEX_POINT('',#8167);
#2393=VERTEX_POINT('',#8169);
#2394=VERTEX_POINT('',#8171);
#2395=VERTEX_POINT('',#8175);
#2396=VERTEX_POINT('',#8179);
#2397=VERTEX_POINT('',#8183);
#2398=VERTEX_POINT('',#8187);
#2399=VERTEX_POINT('',#8202);
#2400=VERTEX_POINT('',#8204);
#2401=VERTEX_POINT('',#8216);
#2402=VERTEX_POINT('',#8219);
#2403=VERTEX_POINT('',#8223);
#2404=VERTEX_POINT('',#8227);
#2405=VERTEX_POINT('',#8231);
#2406=VERTEX_POINT('',#8234);
#2407=VERTEX_POINT('',#8238);
#2408=VERTEX_POINT('',#8242);
#2409=VERTEX_POINT('',#8247);
#2410=VERTEX_POINT('',#8248);
#2411=VERTEX_POINT('',#8250);
#2412=VERTEX_POINT('',#8252);
#2413=VERTEX_POINT('',#8256);
#2414=VERTEX_POINT('',#8258);
#2415=VERTEX_POINT('',#8262);
#2416=VERTEX_POINT('',#8264);
#2417=VERTEX_POINT('',#8268);
#2418=VERTEX_POINT('',#8270);
#2419=VERTEX_POINT('',#8274);
#2420=VERTEX_POINT('',#8276);
#2421=VERTEX_POINT('',#8312);
#2422=VERTEX_POINT('',#8314);
#2423=VERTEX_POINT('',#8318);
#2424=VERTEX_POINT('',#8320);
#2425=VERTEX_POINT('',#8324);
#2426=VERTEX_POINT('',#8326);
#2427=VERTEX_POINT('',#8330);
#2428=VERTEX_POINT('',#8332);
#2429=VERTEX_POINT('',#8336);
#2430=VERTEX_POINT('',#8338);
#2431=VERTEX_POINT('',#8342);
#2432=VERTEX_POINT('',#8346);
#2433=VERTEX_POINT('',#8350);
#2434=VERTEX_POINT('',#8353);
#2435=VERTEX_POINT('',#8355);
#2436=VERTEX_POINT('',#8360);
#2437=VERTEX_POINT('',#8364);
#2438=VERTEX_POINT('',#8366);
#2439=VERTEX_POINT('',#8370);
#2440=VERTEX_POINT('',#8377);
#2441=VERTEX_POINT('',#8379);
#2442=VERTEX_POINT('',#8383);
#2443=VERTEX_POINT('',#8385);
#2444=VERTEX_POINT('',#8392);
#2445=VERTEX_POINT('',#8394);
#2446=VERTEX_POINT('',#8398);
#2447=VERTEX_POINT('',#8400);
#2448=VERTEX_POINT('',#8404);
#2449=VERTEX_POINT('',#8406);
#2450=VERTEX_POINT('',#8410);
#2451=VERTEX_POINT('',#8412);
#2452=VERTEX_POINT('',#8416);
#2453=VERTEX_POINT('',#8418);
#2454=VERTEX_POINT('',#8422);
#2455=VERTEX_POINT('',#8425);
#2456=VERTEX_POINT('',#8429);
#2457=VERTEX_POINT('',#8431);
#2458=VERTEX_POINT('',#8438);
#2459=VERTEX_POINT('',#8440);
#2460=VERTEX_POINT('',#8444);
#2461=VERTEX_POINT('',#8446);
#2462=VERTEX_POINT('',#8450);
#2463=VERTEX_POINT('',#8452);
#2464=VERTEX_POINT('',#8456);
#2465=VERTEX_POINT('',#8458);
#2466=VERTEX_POINT('',#8462);
#2467=VERTEX_POINT('',#8464);
#2468=VERTEX_POINT('',#8468);
#2469=VERTEX_POINT('',#8471);
#2470=VERTEX_POINT('',#8475);
#2471=VERTEX_POINT('',#8477);
#2472=VERTEX_POINT('',#8485);
#2473=VERTEX_POINT('',#8486);
#2474=VERTEX_POINT('',#8489);
#2475=VERTEX_POINT('',#8491);
#2476=VERTEX_POINT('',#8495);
#2477=VERTEX_POINT('',#8499);
#2478=VERTEX_POINT('',#8501);
#2479=VERTEX_POINT('',#8505);
#2480=VERTEX_POINT('',#8510);
#2481=VERTEX_POINT('',#8514);
#2482=VERTEX_POINT('',#8520);
#2483=VERTEX_POINT('',#8521);
#2484=VERTEX_POINT('',#8524);
#2485=VERTEX_POINT('',#8526);
#2486=VERTEX_POINT('',#8530);
#2487=VERTEX_POINT('',#8534);
#2488=VERTEX_POINT('',#8536);
#2489=VERTEX_POINT('',#8539);
#2490=VERTEX_POINT('',#8543);
#2491=VERTEX_POINT('',#8547);
#2492=VERTEX_POINT('',#8555);
#2493=VERTEX_POINT('',#8556);
#2494=VERTEX_POINT('',#8559);
#2495=VERTEX_POINT('',#8560);
#2496=VERTEX_POINT('',#8563);
#2497=VERTEX_POINT('',#8564);
#2498=VERTEX_POINT('',#8567);
#2499=VERTEX_POINT('',#8568);
#2500=VERTEX_POINT('',#8571);
#2501=VERTEX_POINT('',#8572);
#2502=VERTEX_POINT('',#8575);
#2503=VERTEX_POINT('',#8576);
#2504=VERTEX_POINT('',#8579);
#2505=VERTEX_POINT('',#8580);
#2506=VERTEX_POINT('',#8583);
#2507=VERTEX_POINT('',#8584);
#2508=VERTEX_POINT('',#8588);
#2509=VERTEX_POINT('',#8589);
#2510=VERTEX_POINT('',#8612);
#2511=VERTEX_POINT('',#8614);
#2512=VERTEX_POINT('',#8639);
#2513=VERTEX_POINT('',#8641);
#2514=VERTEX_POINT('',#8664);
#2515=VERTEX_POINT('',#8666);
#2516=VERTEX_POINT('',#8689);
#2517=VERTEX_POINT('',#8691);
#2518=VERTEX_POINT('',#8704);
#2519=VERTEX_POINT('',#8707);
#2520=VERTEX_POINT('',#8720);
#2521=VERTEX_POINT('',#8722);
#2522=VERTEX_POINT('',#8745);
#2523=VERTEX_POINT('',#8747);
#2524=VERTEX_POINT('',#8770);
#2525=VERTEX_POINT('',#8772);
#2526=VERTEX_POINT('',#8795);
#2527=VERTEX_POINT('',#8797);
#2528=VERTEX_POINT('',#8822);
#2529=VERTEX_POINT('',#8826);
#2530=VERTEX_POINT('',#8851);
#2531=VERTEX_POINT('',#8855);
#2532=VERTEX_POINT('',#8880);
#2533=VERTEX_POINT('',#8884);
#2534=VERTEX_POINT('',#8885);
#2535=VERTEX_POINT('',#8912);
#2536=VERTEX_POINT('',#8916);
#2537=VERTEX_POINT('',#8941);
#2538=VERTEX_POINT('',#8945);
#2539=VERTEX_POINT('',#8970);
#2540=VERTEX_POINT('',#8974);
#2541=VERTEX_POINT('',#8999);
#2542=VERTEX_POINT('',#9002);
#2543=VERTEX_POINT('',#9004);
#2544=VERTEX_POINT('',#9036);
#2545=VERTEX_POINT('',#9038);
#2546=VERTEX_POINT('',#9041);
#2547=VERTEX_POINT('',#9045);
#2548=VERTEX_POINT('',#9050);
#2549=VERTEX_POINT('',#9052);
#2550=VERTEX_POINT('',#9055);
#2551=VERTEX_POINT('',#9059);
#2552=VERTEX_POINT('',#9070);
#2553=VERTEX_POINT('',#9071);
#2554=VERTEX_POINT('',#9073);
#2555=VERTEX_POINT('',#9075);
#2556=VERTEX_POINT('',#9079);
#2557=VERTEX_POINT('',#9081);
#2558=VERTEX_POINT('',#9085);
#2559=VERTEX_POINT('',#9087);
#2560=VERTEX_POINT('',#9091);
#2561=VERTEX_POINT('',#9093);
#2562=VERTEX_POINT('',#9097);
#2563=VERTEX_POINT('',#9099);
#2564=VERTEX_POINT('',#9108);
#2565=VERTEX_POINT('',#9111);
#2566=VERTEX_POINT('',#9114);
#2567=VERTEX_POINT('',#9118);
#2568=VERTEX_POINT('',#9122);
#2569=VERTEX_POINT('',#9126);
#2570=VERTEX_POINT('',#9129);
#2571=VERTEX_POINT('',#9151);
#2572=VERTEX_POINT('',#9153);
#2573=VERTEX_POINT('',#9156);
#2574=VERTEX_POINT('',#9158);
#2575=VERTEX_POINT('',#9163);
#2576=VERTEX_POINT('',#9165);
#2577=VERTEX_POINT('',#9167);
#2578=VERTEX_POINT('',#9171);
#2579=VERTEX_POINT('',#9176);
#2580=VERTEX_POINT('',#9178);
#2581=VERTEX_POINT('',#9182);
#2582=VERTEX_POINT('',#9184);
#2583=VERTEX_POINT('',#9188);
#2584=VERTEX_POINT('',#9189);
#2585=VERTEX_POINT('',#9194);
#2586=VERTEX_POINT('',#9195);
#2587=VERTEX_POINT('',#9197);
#2588=VERTEX_POINT('',#9199);
#2589=VERTEX_POINT('',#9204);
#2590=VERTEX_POINT('',#9206);
#2591=VERTEX_POINT('',#9210);
#2592=VERTEX_POINT('',#9215);
#2593=VERTEX_POINT('',#9224);
#2594=VERTEX_POINT('',#9226);
#2595=VERTEX_POINT('',#9230);
#2596=VERTEX_POINT('',#9232);
#2597=VERTEX_POINT('',#9239);
#2598=VERTEX_POINT('',#9241);
#2599=VERTEX_POINT('',#9245);
#2600=VERTEX_POINT('',#9246);
#2601=VERTEX_POINT('',#9248);
#2602=VERTEX_POINT('',#9250);
#2603=VERTEX_POINT('',#9254);
#2604=VERTEX_POINT('',#9256);
#2605=VERTEX_POINT('',#9260);
#2606=VERTEX_POINT('',#9262);
#2607=VERTEX_POINT('',#9266);
#2608=VERTEX_POINT('',#9268);
#2609=VERTEX_POINT('',#9272);
#2610=VERTEX_POINT('',#9274);
#2611=VERTEX_POINT('',#9288);
#2612=VERTEX_POINT('',#9290);
#2613=VERTEX_POINT('',#9294);
#2614=VERTEX_POINT('',#9296);
#2615=VERTEX_POINT('',#9300);
#2616=VERTEX_POINT('',#9301);
#2617=VERTEX_POINT('',#9303);
#2618=VERTEX_POINT('',#9305);
#2619=EDGE_CURVE('',#2208,#2209,#1915,.T.);
#2620=EDGE_CURVE('',#2208,#2210,#1916,.T.);
#2621=EDGE_CURVE('',#2211,#2210,#1917,.T.);
#2622=EDGE_CURVE('',#2211,#2212,#1918,.T.);
#2623=EDGE_CURVE('',#2213,#2212,#1919,.T.);
#2624=EDGE_CURVE('',#2213,#2214,#1920,.T.);
#2625=EDGE_CURVE('',#2215,#2214,#1921,.T.);
#2626=EDGE_CURVE('',#2215,#2209,#1922,.T.);
#2627=EDGE_CURVE('',#2216,#2216,#1923,.T.);
#2628=EDGE_CURVE('',#2214,#2217,#424,.T.);
#2629=EDGE_CURVE('',#2218,#2213,#425,.T.);
#2630=EDGE_CURVE('',#2217,#2218,#1924,.T.);
#2631=EDGE_CURVE('',#2219,#2211,#426,.T.);
#2632=EDGE_CURVE('',#2220,#2219,#1925,.T.);
#2633=EDGE_CURVE('',#2212,#2220,#427,.T.);
#2634=EDGE_CURVE('',#2209,#2221,#428,.T.);
#2635=EDGE_CURVE('',#2222,#2215,#429,.T.);
#2636=EDGE_CURVE('',#2221,#2222,#1926,.T.);
#2637=EDGE_CURVE('',#2216,#2223,#430,.T.);
#2638=EDGE_CURVE('',#2223,#2223,#1927,.T.);
#2639=EDGE_CURVE('',#2224,#2208,#431,.T.);
#2640=EDGE_CURVE('',#2225,#2224,#1928,.T.);
#2641=EDGE_CURVE('',#2210,#2225,#432,.T.);
#2642=EDGE_CURVE('',#2226,#2226,#1929,.T.);
#2643=EDGE_CURVE('',#2226,#2227,#433,.T.);
#2644=EDGE_CURVE('',#2224,#2227,#1930,.T.);
#2645=EDGE_CURVE('',#2227,#2221,#1931,.T.);
#2646=EDGE_CURVE('',#2228,#2228,#1932,.T.);
#2647=EDGE_CURVE('',#2228,#2229,#434,.T.);
#2648=EDGE_CURVE('',#2222,#2229,#1933,.T.);
#2649=EDGE_CURVE('',#2229,#2217,#1934,.T.);
#2650=EDGE_CURVE('',#2230,#2230,#1935,.T.);
#2651=EDGE_CURVE('',#2230,#2231,#435,.T.);
#2652=EDGE_CURVE('',#2218,#2231,#1936,.T.);
#2653=EDGE_CURVE('',#2231,#2220,#1937,.T.);
#2654=EDGE_CURVE('',#2232,#2232,#1938,.T.);
#2655=EDGE_CURVE('',#2233,#2233,#1939,.T.);
#2656=EDGE_CURVE('',#2233,#2234,#436,.T.);
#2657=EDGE_CURVE('',#2219,#2234,#1940,.T.);
#2658=EDGE_CURVE('',#2234,#2225,#1941,.T.);
#2659=EDGE_CURVE('',#2235,#2235,#1942,.T.);
#2660=EDGE_CURVE('',#2235,#2236,#437,.T.);
#2661=EDGE_CURVE('',#2236,#2236,#1943,.T.);
#2662=EDGE_CURVE('',#2237,#2237,#1944,.T.);
#2663=EDGE_CURVE('',#2237,#2238,#438,.T.);
#2664=EDGE_CURVE('',#2238,#2238,#1945,.T.);
#2665=EDGE_CURVE('',#2239,#2239,#1946,.T.);
#2666=EDGE_CURVE('',#2239,#2240,#439,.T.);
#2667=EDGE_CURVE('',#2240,#2240,#1947,.T.);
#2668=EDGE_CURVE('',#2241,#2241,#1948,.T.);
#2669=EDGE_CURVE('',#2241,#2232,#440,.T.);
#2670=EDGE_CURVE('',#2242,#2243,#441,.T.);
#2671=EDGE_CURVE('',#2242,#2244,#442,.T.);
#2672=EDGE_CURVE('',#2245,#2244,#443,.T.);
#2673=EDGE_CURVE('',#2243,#2245,#444,.T.);
#2674=EDGE_CURVE('',#2243,#2246,#445,.T.);
#2675=EDGE_CURVE('',#2247,#2245,#446,.T.);
#2676=EDGE_CURVE('',#2246,#2247,#447,.T.);
#2677=EDGE_CURVE('',#2246,#2248,#448,.T.);
#2678=EDGE_CURVE('',#2249,#2247,#449,.T.);
#2679=EDGE_CURVE('',#2248,#2249,#450,.T.);
#2680=EDGE_CURVE('',#2248,#2250,#451,.T.);
#2681=EDGE_CURVE('',#2251,#2249,#452,.T.);
#2682=EDGE_CURVE('',#2250,#2251,#453,.T.);
#2683=EDGE_CURVE('',#2250,#2252,#454,.T.);
#2684=EDGE_CURVE('',#2253,#2251,#455,.T.);
#2685=EDGE_CURVE('',#2252,#2253,#456,.T.);
#2686=EDGE_CURVE('',#2252,#2254,#457,.T.);
#2687=EDGE_CURVE('',#2255,#2253,#458,.T.);
#2688=EDGE_CURVE('',#2254,#2255,#459,.T.);
#2689=EDGE_CURVE('',#2254,#2256,#460,.T.);
#2690=EDGE_CURVE('',#2257,#2255,#461,.T.);
#2691=EDGE_CURVE('',#2256,#2257,#462,.T.);
#2692=EDGE_CURVE('',#2256,#2242,#463,.T.);
#2693=EDGE_CURVE('',#2244,#2257,#464,.T.);
#2694=EDGE_CURVE('',#2258,#2259,#1949,.T.);
#2695=EDGE_CURVE('',#2260,#2258,#1950,.T.);
#2696=EDGE_CURVE('',#2261,#2260,#1951,.T.);
#2697=EDGE_CURVE('',#2262,#2261,#1952,.T.);
#2698=EDGE_CURVE('',#2263,#2262,#1953,.T.);
#2699=EDGE_CURVE('',#2264,#2263,#1954,.T.);
#2700=EDGE_CURVE('',#2265,#2264,#1955,.T.);
#2701=EDGE_CURVE('',#2259,#2265,#1956,.T.);
#2702=EDGE_CURVE('',#2266,#2266,#1957,.T.);
#2703=EDGE_CURVE('',#2264,#2267,#465,.T.);
#2704=EDGE_CURVE('',#2268,#2263,#466,.T.);
#2705=EDGE_CURVE('',#2267,#2268,#1958,.T.);
#2706=EDGE_CURVE('',#2259,#2269,#467,.T.);
#2707=EDGE_CURVE('',#2270,#2265,#468,.T.);
#2708=EDGE_CURVE('',#2269,#2270,#1959,.T.);
#2709=EDGE_CURVE('',#2271,#2261,#469,.T.);
#2710=EDGE_CURVE('',#2272,#2271,#1960,.T.);
#2711=EDGE_CURVE('',#2262,#2272,#470,.T.);
#2712=EDGE_CURVE('',#2273,#2273,#1961,.T.);
#2713=EDGE_CURVE('',#2273,#2266,#471,.T.);
#2714=EDGE_CURVE('',#2274,#2258,#472,.T.);
#2715=EDGE_CURVE('',#2275,#2274,#1962,.T.);
#2716=EDGE_CURVE('',#2260,#2275,#473,.T.);
#2717=EDGE_CURVE('',#2276,#2269,#1963,.T.);
#2718=EDGE_CURVE('',#2276,#2277,#474,.T.);
#2719=EDGE_CURVE('',#2277,#2277,#1964,.T.);
#2720=EDGE_CURVE('',#2274,#2276,#1965,.T.);
#2721=EDGE_CURVE('',#2278,#2267,#1966,.T.);
#2722=EDGE_CURVE('',#2278,#2279,#475,.T.);
#2723=EDGE_CURVE('',#2279,#2279,#1967,.T.);
#2724=EDGE_CURVE('',#2270,#2278,#1968,.T.);
#2725=EDGE_CURVE('',#2280,#2280,#1969,.T.);
#2726=EDGE_CURVE('',#2281,#2275,#1970,.T.);
#2727=EDGE_CURVE('',#2281,#2282,#476,.T.);
#2728=EDGE_CURVE('',#2282,#2282,#1971,.T.);
#2729=EDGE_CURVE('',#2271,#2281,#1972,.T.);
#2730=EDGE_CURVE('',#2283,#2272,#1973,.T.);
#2731=EDGE_CURVE('',#2283,#2284,#477,.T.);
#2732=EDGE_CURVE('',#2284,#2284,#1974,.T.);
#2733=EDGE_CURVE('',#2268,#2283,#1975,.T.);
#2734=EDGE_CURVE('',#2285,#2285,#1976,.T.);
#2735=EDGE_CURVE('',#2285,#2286,#478,.T.);
#2736=EDGE_CURVE('',#2286,#2286,#1977,.T.);
#2737=EDGE_CURVE('',#2287,#2287,#1978,.T.);
#2738=EDGE_CURVE('',#2287,#2288,#479,.T.);
#2739=EDGE_CURVE('',#2288,#2288,#1979,.T.);
#2740=EDGE_CURVE('',#2289,#2289,#1980,.T.);
#2741=EDGE_CURVE('',#2289,#2290,#480,.T.);
#2742=EDGE_CURVE('',#2290,#2290,#1981,.T.);
#2743=EDGE_CURVE('',#2280,#2291,#481,.T.);
#2744=EDGE_CURVE('',#2291,#2291,#1982,.T.);
#2745=EDGE_CURVE('',#2292,#2293,#482,.T.);
#2746=EDGE_CURVE('',#2292,#2294,#483,.T.);
#2747=EDGE_CURVE('',#2295,#2294,#484,.T.);
#2748=EDGE_CURVE('',#2293,#2295,#485,.T.);
#2749=EDGE_CURVE('',#2293,#2296,#486,.T.);
#2750=EDGE_CURVE('',#2297,#2295,#487,.T.);
#2751=EDGE_CURVE('',#2296,#2297,#488,.T.);
#2752=EDGE_CURVE('',#2296,#2298,#489,.T.);
#2753=EDGE_CURVE('',#2299,#2297,#490,.T.);
#2754=EDGE_CURVE('',#2298,#2299,#491,.T.);
#2755=EDGE_CURVE('',#2298,#2300,#492,.T.);
#2756=EDGE_CURVE('',#2301,#2299,#493,.T.);
#2757=EDGE_CURVE('',#2300,#2301,#494,.T.);
#2758=EDGE_CURVE('',#2300,#2302,#495,.T.);
#2759=EDGE_CURVE('',#2303,#2301,#496,.T.);
#2760=EDGE_CURVE('',#2302,#2303,#497,.T.);
#2761=EDGE_CURVE('',#2302,#2304,#498,.T.);
#2762=EDGE_CURVE('',#2305,#2303,#499,.T.);
#2763=EDGE_CURVE('',#2304,#2305,#500,.T.);
#2764=EDGE_CURVE('',#2304,#2306,#501,.T.);
#2765=EDGE_CURVE('',#2307,#2305,#502,.T.);
#2766=EDGE_CURVE('',#2306,#2307,#503,.T.);
#2767=EDGE_CURVE('',#2306,#2292,#504,.T.);
#2768=EDGE_CURVE('',#2294,#2307,#505,.T.);
#2769=EDGE_CURVE('',#2308,#2308,#1983,.T.);
#2770=EDGE_CURVE('',#2308,#2309,#506,.T.);
#2771=EDGE_CURVE('',#2309,#2309,#1984,.T.);
#2772=EDGE_CURVE('',#2310,#2310,#1985,.T.);
#2773=EDGE_CURVE('',#2310,#2311,#507,.T.);
#2774=EDGE_CURVE('',#2311,#2311,#1986,.T.);
#2775=EDGE_CURVE('',#2312,#2312,#1987,.T.);
#2776=EDGE_CURVE('',#2312,#2313,#508,.T.);
#2777=EDGE_CURVE('',#2313,#2313,#1988,.T.);
#2778=EDGE_CURVE('',#2314,#2315,#509,.T.);
#2779=EDGE_CURVE('',#2315,#2316,#510,.T.);
#2780=EDGE_CURVE('',#2317,#2316,#511,.T.);
#2781=EDGE_CURVE('',#2314,#2317,#512,.T.);
#2782=EDGE_CURVE('',#2318,#2314,#513,.T.);
#2783=EDGE_CURVE('',#2319,#2317,#514,.T.);
#2784=EDGE_CURVE('',#2318,#2319,#515,.T.);
#2785=EDGE_CURVE('',#2320,#2318,#516,.T.);
#2786=EDGE_CURVE('',#2321,#2319,#517,.T.);
#2787=EDGE_CURVE('',#2320,#2321,#518,.T.);
#2788=EDGE_CURVE('',#2315,#2320,#519,.T.);
#2789=EDGE_CURVE('',#2316,#2321,#520,.T.);
#2790=EDGE_CURVE('',#2322,#2322,#1989,.T.);
#2791=EDGE_CURVE('',#2322,#2323,#521,.T.);
#2792=EDGE_CURVE('',#2323,#2323,#1990,.T.);
#2793=EDGE_CURVE('',#2324,#2324,#1991,.T.);
#2794=EDGE_CURVE('',#2324,#2325,#522,.T.);
#2795=EDGE_CURVE('',#2325,#2325,#1992,.T.);
#2796=EDGE_CURVE('',#2326,#2326,#1993,.T.);
#2797=EDGE_CURVE('',#2326,#2327,#523,.T.);
#2798=EDGE_CURVE('',#2327,#2327,#1994,.T.);
#2799=EDGE_CURVE('',#2328,#2328,#1995,.T.);
#2800=EDGE_CURVE('',#2329,#2329,#1996,.T.);
#2801=EDGE_CURVE('',#2328,#2330,#524,.T.);
#2802=EDGE_CURVE('',#2330,#2330,#1997,.T.);
#2803=EDGE_CURVE('',#2331,#2331,#1998,.T.);
#2804=EDGE_CURVE('',#2331,#2329,#525,.T.);
#2805=EDGE_CURVE('',#2332,#2332,#1999,.T.);
#2806=EDGE_CURVE('',#2332,#2333,#526,.T.);
#2807=EDGE_CURVE('',#2333,#2333,#2000,.T.);
#2808=EDGE_CURVE('',#2334,#2334,#2001,.T.);
#2809=EDGE_CURVE('',#2334,#2335,#527,.T.);
#2810=EDGE_CURVE('',#2335,#2335,#2002,.T.);
#2811=EDGE_CURVE('',#2336,#2336,#2003,.T.);
#2812=EDGE_CURVE('',#2336,#2337,#528,.T.);
#2813=EDGE_CURVE('',#2337,#2337,#2004,.T.);
#2814=EDGE_CURVE('',#2338,#2338,#2005,.T.);
#2815=EDGE_CURVE('',#2338,#2339,#529,.T.);
#2816=EDGE_CURVE('',#2339,#2339,#2006,.T.);
#2817=EDGE_CURVE('',#2340,#2340,#2007,.T.);
#2818=EDGE_CURVE('',#2340,#2341,#530,.T.);
#2819=EDGE_CURVE('',#2341,#2341,#2008,.T.);
#2820=EDGE_CURVE('',#2342,#2342,#2009,.T.);
#2821=EDGE_CURVE('',#2342,#2343,#531,.T.);
#2822=EDGE_CURVE('',#2343,#2343,#2010,.T.);
#2823=EDGE_CURVE('',#2344,#2344,#2011,.T.);
#2824=EDGE_CURVE('',#2344,#2345,#532,.T.);
#2825=EDGE_CURVE('',#2345,#2345,#2012,.T.);
#2826=EDGE_CURVE('',#2346,#2346,#2013,.T.);
#2827=EDGE_CURVE('',#2346,#2347,#533,.T.);
#2828=EDGE_CURVE('',#2347,#2347,#2014,.T.);
#2829=EDGE_CURVE('',#2348,#2348,#2015,.T.);
#2830=EDGE_CURVE('',#2348,#2349,#534,.T.);
#2831=EDGE_CURVE('',#2349,#2349,#2016,.T.);
#2832=EDGE_CURVE('',#2350,#2350,#2017,.T.);
#2833=EDGE_CURVE('',#2350,#2351,#535,.T.);
#2834=EDGE_CURVE('',#2351,#2351,#2018,.T.);
#2835=EDGE_CURVE('',#2352,#2352,#2019,.T.);
#2836=EDGE_CURVE('',#2352,#2353,#536,.T.);
#2837=EDGE_CURVE('',#2353,#2353,#2020,.T.);
#2838=EDGE_CURVE('',#2354,#2354,#2021,.T.);
#2839=EDGE_CURVE('',#2354,#2355,#537,.T.);
#2840=EDGE_CURVE('',#2355,#2355,#2022,.T.);
#2841=EDGE_CURVE('',#2356,#2356,#2023,.T.);
#2842=EDGE_CURVE('',#2356,#2357,#538,.T.);
#2843=EDGE_CURVE('',#2357,#2357,#2024,.T.);
#2844=EDGE_CURVE('',#2358,#2358,#2025,.T.);
#2845=EDGE_CURVE('',#2358,#2359,#539,.T.);
#2846=EDGE_CURVE('',#2359,#2359,#2026,.T.);
#2847=EDGE_CURVE('',#2360,#2361,#540,.T.);
#2848=EDGE_CURVE('',#2361,#2362,#541,.T.);
#2849=EDGE_CURVE('',#2362,#2363,#542,.T.);
#2850=EDGE_CURVE('',#2360,#2363,#543,.T.);
#2851=EDGE_CURVE('',#2361,#2364,#544,.T.);
#2852=EDGE_CURVE('',#2364,#2365,#545,.T.);
#2853=EDGE_CURVE('',#2365,#2362,#546,.T.);
#2854=EDGE_CURVE('',#2364,#2366,#547,.T.);
#2855=EDGE_CURVE('',#2366,#2367,#548,.T.);
#2856=EDGE_CURVE('',#2367,#2365,#549,.T.);
#2857=EDGE_CURVE('',#2366,#2368,#550,.T.);
#2858=EDGE_CURVE('',#2368,#2369,#551,.T.);
#2859=EDGE_CURVE('',#2369,#2367,#552,.T.);
#2860=EDGE_CURVE('',#2368,#2370,#553,.T.);
#2861=EDGE_CURVE('',#2370,#2371,#554,.T.);
#2862=EDGE_CURVE('',#2371,#2369,#555,.T.);
#2863=EDGE_CURVE('',#2370,#2360,#556,.T.);
#2864=EDGE_CURVE('',#2363,#2371,#557,.T.);
#2865=EDGE_CURVE('',#2372,#2372,#2027,.T.);
#2866=EDGE_CURVE('',#2373,#2373,#2028,.T.);
#2867=EDGE_CURVE('',#2372,#2374,#558,.T.);
#2868=EDGE_CURVE('',#2374,#2374,#2029,.T.);
#2869=EDGE_CURVE('',#2375,#2375,#2030,.T.);
#2870=EDGE_CURVE('',#2376,#2376,#2031,.T.);
#2871=EDGE_CURVE('',#2376,#2375,#559,.T.);
#2872=EDGE_CURVE('',#2377,#2377,#2032,.T.);
#2873=EDGE_CURVE('',#2377,#2376,#560,.T.);
#2874=EDGE_CURVE('',#2378,#2378,#2033,.T.);
#2875=EDGE_CURVE('',#2378,#2377,#561,.T.);
#2876=EDGE_CURVE('',#2379,#2379,#2034,.T.);
#2877=EDGE_CURVE('',#2380,#2380,#2035,.F.);
#2878=EDGE_CURVE('',#2380,#2379,#562,.T.);
#2879=EDGE_CURVE('',#2373,#2380,#563,.T.);
#2880=EDGE_CURVE('',#2381,#2381,#2036,.T.);
#2881=EDGE_CURVE('',#2381,#2382,#564,.T.);
#2882=EDGE_CURVE('',#2382,#2382,#2037,.T.);
#2883=EDGE_CURVE('',#2383,#2383,#2038,.T.);
#2884=EDGE_CURVE('',#2383,#2384,#565,.T.);
#2885=EDGE_CURVE('',#2384,#2384,#2039,.T.);
#2886=EDGE_CURVE('',#2385,#2386,#255,.T.);
#2887=EDGE_CURVE('',#2387,#2385,#256,.T.);
#2888=EDGE_CURVE('',#2387,#2388,#566,.T.);
#2889=EDGE_CURVE('',#2388,#2388,#2040,.T.);
#2890=EDGE_CURVE('',#2389,#2387,#257,.T.);
#2891=EDGE_CURVE('',#2390,#2389,#258,.T.);
#2892=EDGE_CURVE('',#2391,#2390,#259,.T.);
#2893=EDGE_CURVE('',#2386,#2391,#260,.T.);
#2894=EDGE_CURVE('',#2392,#2392,#2041,.T.);
#2895=EDGE_CURVE('',#2392,#2393,#567,.T.);
#2896=EDGE_CURVE('',#2394,#2393,#261,.T.);
#2897=EDGE_CURVE('',#2395,#2394,#262,.T.);
#2898=EDGE_CURVE('',#2396,#2395,#263,.T.);
#2899=EDGE_CURVE('',#2397,#2396,#264,.T.);
#2900=EDGE_CURVE('',#2398,#2397,#265,.T.);
#2901=EDGE_CURVE('',#2393,#2398,#266,.T.);
#2902=EDGE_CURVE('',#2389,#2398,#568,.T.);
#2903=EDGE_CURVE('',#2390,#2397,#569,.T.);
#2904=EDGE_CURVE('',#2387,#2393,#570,.T.);
#2905=EDGE_CURVE('',#2385,#2394,#571,.T.);
#2906=EDGE_CURVE('',#2399,#2399,#2042,.F.);
#2907=EDGE_CURVE('',#2399,#2400,#572,.T.);
#2908=EDGE_CURVE('',#2400,#2400,#2043,.F.);
#2909=EDGE_CURVE('',#2386,#2395,#573,.T.);
#2910=EDGE_CURVE('',#2391,#2396,#574,.T.);
#2911=EDGE_CURVE('',#2401,#2401,#2044,.T.);
#2912=EDGE_CURVE('',#2402,#2402,#2045,.T.);
#2913=EDGE_CURVE('',#2402,#2401,#575,.T.);
#2914=EDGE_CURVE('',#2403,#2403,#2046,.T.);
#2915=EDGE_CURVE('',#2403,#2402,#576,.T.);
#2916=EDGE_CURVE('',#2404,#2404,#2047,.T.);
#2917=EDGE_CURVE('',#2404,#2403,#577,.T.);
#2918=EDGE_CURVE('',#2405,#2405,#2048,.T.);
#2919=EDGE_CURVE('',#2406,#2406,#2049,.F.);
#2920=EDGE_CURVE('',#2406,#2405,#578,.T.);
#2921=EDGE_CURVE('',#2407,#2407,#2050,.F.);
#2922=EDGE_CURVE('',#2407,#2406,#579,.T.);
#2923=EDGE_CURVE('',#2408,#2408,#2051,.T.);
#2924=EDGE_CURVE('',#2408,#2407,#580,.T.);
#2925=EDGE_CURVE('',#2409,#2410,#581,.T.);
#2926=EDGE_CURVE('',#2410,#2411,#582,.T.);
#2927=EDGE_CURVE('',#2411,#2412,#583,.T.);
#2928=EDGE_CURVE('',#2409,#2412,#584,.T.);
#2929=EDGE_CURVE('',#2410,#2413,#585,.T.);
#2930=EDGE_CURVE('',#2413,#2414,#586,.T.);
#2931=EDGE_CURVE('',#2414,#2411,#587,.T.);
#2932=EDGE_CURVE('',#2413,#2415,#588,.T.);
#2933=EDGE_CURVE('',#2415,#2416,#589,.T.);
#2934=EDGE_CURVE('',#2416,#2414,#590,.T.);
#2935=EDGE_CURVE('',#2415,#2417,#591,.T.);
#2936=EDGE_CURVE('',#2417,#2418,#592,.T.);
#2937=EDGE_CURVE('',#2418,#2416,#593,.T.);
#2938=EDGE_CURVE('',#2417,#2419,#594,.T.);
#2939=EDGE_CURVE('',#2419,#2420,#595,.T.);
#2940=EDGE_CURVE('',#2420,#2418,#596,.T.);
#2941=EDGE_CURVE('',#2419,#2409,#597,.T.);
#2942=EDGE_CURVE('',#2412,#2420,#598,.T.);
#2943=EDGE_CURVE('',#2421,#2421,#2052,.T.);
#2944=EDGE_CURVE('',#2421,#2422,#599,.T.);
#2945=EDGE_CURVE('',#2422,#2422,#2053,.T.);
#2946=EDGE_CURVE('',#2423,#2423,#2054,.T.);
#2947=EDGE_CURVE('',#2423,#2424,#600,.T.);
#2948=EDGE_CURVE('',#2424,#2424,#2055,.T.);
#2949=EDGE_CURVE('',#2425,#2425,#2056,.T.);
#2950=EDGE_CURVE('',#2425,#2426,#601,.T.);
#2951=EDGE_CURVE('',#2426,#2426,#2057,.T.);
#2952=EDGE_CURVE('',#2427,#2427,#2058,.T.);
#2953=EDGE_CURVE('',#2427,#2428,#602,.T.);
#2954=EDGE_CURVE('',#2428,#2428,#2059,.T.);
#2955=EDGE_CURVE('',#2429,#2429,#2060,.T.);
#2956=EDGE_CURVE('',#2429,#2430,#603,.T.);
#2957=EDGE_CURVE('',#2430,#2430,#2061,.T.);
#2958=EDGE_CURVE('',#2431,#2431,#2062,.T.);
#2959=EDGE_CURVE('',#2431,#2429,#604,.T.);
#2960=EDGE_CURVE('',#2432,#2432,#2063,.T.);
#2961=EDGE_CURVE('',#2432,#2431,#605,.T.);
#2962=EDGE_CURVE('',#2433,#2433,#2064,.T.);
#2963=EDGE_CURVE('',#2434,#2434,#2065,.T.);
#2964=EDGE_CURVE('',#2435,#2435,#2066,.T.);
#2965=EDGE_CURVE('',#2430,#2434,#606,.T.);
#2966=EDGE_CURVE('',#2435,#2436,#607,.T.);
#2967=EDGE_CURVE('',#2436,#2436,#2067,.T.);
#2968=EDGE_CURVE('',#2437,#2437,#2068,.T.);
#2969=EDGE_CURVE('',#2437,#2438,#608,.T.);
#2970=EDGE_CURVE('',#2438,#2438,#2069,.T.);
#2971=EDGE_CURVE('',#2439,#2439,#2070,.T.);
#2972=EDGE_CURVE('',#2439,#2433,#609,.T.);
#2973=EDGE_CURVE('',#2440,#2440,#2071,.T.);
#2974=EDGE_CURVE('',#2440,#2441,#610,.T.);
#2975=EDGE_CURVE('',#2441,#2441,#2072,.T.);
#2976=EDGE_CURVE('',#2442,#2442,#2073,.T.);
#2977=EDGE_CURVE('',#2442,#2443,#611,.T.);
#2978=EDGE_CURVE('',#2443,#2443,#2074,.T.);
#2979=EDGE_CURVE('',#2444,#2444,#2075,.T.);
#2980=EDGE_CURVE('',#2444,#2445,#612,.T.);
#2981=EDGE_CURVE('',#2445,#2445,#2076,.T.);
#2982=EDGE_CURVE('',#2446,#2446,#2077,.T.);
#2983=EDGE_CURVE('',#2446,#2447,#613,.T.);
#2984=EDGE_CURVE('',#2447,#2447,#2078,.T.);
#2985=EDGE_CURVE('',#2448,#2448,#2079,.T.);
#2986=EDGE_CURVE('',#2448,#2449,#614,.T.);
#2987=EDGE_CURVE('',#2449,#2449,#2080,.T.);
#2988=EDGE_CURVE('',#2450,#2450,#2081,.T.);
#2989=EDGE_CURVE('',#2450,#2451,#615,.T.);
#2990=EDGE_CURVE('',#2451,#2451,#2082,.T.);
#2991=EDGE_CURVE('',#2452,#2452,#2083,.T.);
#2992=EDGE_CURVE('',#2452,#2453,#616,.T.);
#2993=EDGE_CURVE('',#2453,#2453,#2084,.T.);
#2994=EDGE_CURVE('',#2454,#2454,#2085,.T.);
#2995=EDGE_CURVE('',#2454,#2455,#617,.T.);
#2996=EDGE_CURVE('',#2455,#2455,#2086,.T.);
#2997=EDGE_CURVE('',#2456,#2456,#2087,.T.);
#2998=EDGE_CURVE('',#2456,#2457,#618,.T.);
#2999=EDGE_CURVE('',#2457,#2457,#2088,.T.);
#3000=EDGE_CURVE('',#2458,#2458,#2089,.T.);
#3001=EDGE_CURVE('',#2458,#2459,#619,.T.);
#3002=EDGE_CURVE('',#2459,#2459,#2090,.T.);
#3003=EDGE_CURVE('',#2460,#2460,#2091,.T.);
#3004=EDGE_CURVE('',#2460,#2461,#620,.T.);
#3005=EDGE_CURVE('',#2461,#2461,#2092,.T.);
#3006=EDGE_CURVE('',#2462,#2462,#2093,.T.);
#3007=EDGE_CURVE('',#2462,#2463,#621,.T.);
#3008=EDGE_CURVE('',#2463,#2463,#2094,.T.);
#3009=EDGE_CURVE('',#2464,#2464,#2095,.T.);
#3010=EDGE_CURVE('',#2464,#2465,#622,.T.);
#3011=EDGE_CURVE('',#2465,#2465,#2096,.T.);
#3012=EDGE_CURVE('',#2466,#2466,#2097,.T.);
#3013=EDGE_CURVE('',#2466,#2467,#623,.T.);
#3014=EDGE_CURVE('',#2467,#2467,#2098,.T.);
#3015=EDGE_CURVE('',#2468,#2468,#2099,.T.);
#3016=EDGE_CURVE('',#2469,#2469,#2100,.T.);
#3017=EDGE_CURVE('',#2469,#2468,#624,.T.);
#3018=EDGE_CURVE('',#2470,#2470,#2101,.T.);
#3019=EDGE_CURVE('',#2470,#2471,#625,.T.);
#3020=EDGE_CURVE('',#2471,#2471,#2102,.T.);
#3021=EDGE_CURVE('',#2472,#2473,#2103,.T.);
#3022=EDGE_CURVE('',#2473,#2472,#2104,.T.);
#3023=EDGE_CURVE('',#2473,#2474,#2105,.T.);
#3024=EDGE_CURVE('',#2475,#2474,#2106,.T.);
#3025=EDGE_CURVE('',#2474,#2475,#2107,.T.);
#3026=EDGE_CURVE('',#2475,#2476,#626,.T.);
#3027=EDGE_CURVE('',#2476,#2476,#2108,.T.);
#3028=EDGE_CURVE('',#2477,#2477,#2109,.T.);
#3029=EDGE_CURVE('',#2477,#2478,#627,.T.);
#3030=EDGE_CURVE('',#2478,#2478,#2110,.T.);
#3031=EDGE_CURVE('',#2478,#2479,#628,.T.);
#3032=EDGE_CURVE('',#2479,#2479,#2111,.T.);
#3033=EDGE_CURVE('',#2480,#2480,#2112,.T.);
#3034=EDGE_CURVE('',#2480,#2472,#629,.T.);
#3035=EDGE_CURVE('',#2481,#2481,#2113,.T.);
#3036=EDGE_CURVE('',#2481,#2477,#630,.T.);
#3037=EDGE_CURVE('',#2482,#2483,#2114,.T.);
#3038=EDGE_CURVE('',#2483,#2482,#2115,.T.);
#3039=EDGE_CURVE('',#2483,#2484,#2116,.T.);
#3040=EDGE_CURVE('',#2485,#2484,#2117,.T.);
#3041=EDGE_CURVE('',#2484,#2485,#2118,.T.);
#3042=EDGE_CURVE('',#2486,#2486,#2119,.T.);
#3043=EDGE_CURVE('',#2486,#2485,#631,.T.);
#3044=EDGE_CURVE('',#2487,#2487,#2120,.T.);
#3045=EDGE_CURVE('',#2488,#2488,#2121,.T.);
#3046=EDGE_CURVE('',#2489,#2489,#2122,.T.);
#3047=EDGE_CURVE('',#2489,#2487,#632,.T.);
#3048=EDGE_CURVE('',#2490,#2490,#2123,.T.);
#3049=EDGE_CURVE('',#2490,#2489,#633,.T.);
#3050=EDGE_CURVE('',#2491,#2491,#2124,.T.);
#3051=EDGE_CURVE('',#2491,#2490,#634,.T.);
#3052=EDGE_CURVE('',#2482,#2488,#635,.T.);
#3053=EDGE_CURVE('',#2492,#2493,#2125,.T.);
#3054=EDGE_CURVE('',#2494,#2495,#2126,.T.);
#3055=EDGE_CURVE('',#2496,#2497,#2127,.T.);
#3056=EDGE_CURVE('',#2498,#2499,#2128,.T.);
#3057=EDGE_CURVE('',#2500,#2501,#2129,.T.);
#3058=EDGE_CURVE('',#2502,#2503,#2130,.T.);
#3059=EDGE_CURVE('',#2504,#2505,#2131,.T.);
#3060=EDGE_CURVE('',#2506,#2507,#2132,.T.);
#3061=EDGE_CURVE('',#2508,#2509,#11,.T.);
#3062=EDGE_CURVE('',#2510,#2508,#2133,.T.);
#3063=EDGE_CURVE('',#2511,#2510,#12,.T.);
#3064=EDGE_CURVE('',#2509,#2511,#2134,.T.);
#3065=EDGE_CURVE('',#2512,#2510,#2135,.T.);
#3066=EDGE_CURVE('',#2512,#2513,#13,.T.);
#3067=EDGE_CURVE('',#2514,#2513,#2136,.T.);
#3068=EDGE_CURVE('',#2514,#2515,#14,.T.);
#3069=EDGE_CURVE('',#2516,#2515,#2137,.T.);
#3070=EDGE_CURVE('',#2516,#2517,#15,.T.);
#3071=EDGE_CURVE('',#2517,#2518,#636,.T.);
#3072=EDGE_CURVE('',#2518,#2518,#2138,.T.);
#3073=EDGE_CURVE('',#2517,#2519,#16,.T.);
#3074=EDGE_CURVE('',#2520,#2519,#2139,.T.);
#3075=EDGE_CURVE('',#2520,#2521,#17,.T.);
#3076=EDGE_CURVE('',#2522,#2521,#2140,.T.);
#3077=EDGE_CURVE('',#2522,#2523,#18,.T.);
#3078=EDGE_CURVE('',#2524,#2523,#2141,.T.);
#3079=EDGE_CURVE('',#2524,#2525,#19,.T.);
#3080=EDGE_CURVE('',#2526,#2525,#2142,.T.);
#3081=EDGE_CURVE('',#2526,#2527,#20,.T.);
#3082=EDGE_CURVE('',#2511,#2527,#2143,.T.);
#3083=EDGE_CURVE('',#2508,#2528,#2144,.T.);
#3084=EDGE_CURVE('',#2528,#2512,#2145,.T.);
#3085=EDGE_CURVE('',#2529,#2528,#21,.T.);
#3086=EDGE_CURVE('',#2513,#2529,#2146,.T.);
#3087=EDGE_CURVE('',#2529,#2530,#2147,.T.);
#3088=EDGE_CURVE('',#2530,#2514,#2148,.T.);
#3089=EDGE_CURVE('',#2531,#2530,#22,.T.);
#3090=EDGE_CURVE('',#2515,#2531,#2149,.T.);
#3091=EDGE_CURVE('',#2531,#2532,#2150,.T.);
#3092=EDGE_CURVE('',#2532,#2516,#2151,.T.);
#3093=EDGE_CURVE('',#2533,#2534,#23,.T.);
#3094=EDGE_CURVE('',#2519,#2533,#2152,.T.);
#3095=EDGE_CURVE('',#2534,#2532,#24,.T.);
#3096=EDGE_CURVE('',#2533,#2535,#2153,.T.);
#3097=EDGE_CURVE('',#2535,#2520,#2154,.T.);
#3098=EDGE_CURVE('',#2536,#2535,#25,.T.);
#3099=EDGE_CURVE('',#2521,#2536,#2155,.T.);
#3100=EDGE_CURVE('',#2536,#2537,#2156,.T.);
#3101=EDGE_CURVE('',#2537,#2522,#2157,.T.);
#3102=EDGE_CURVE('',#2538,#2537,#26,.T.);
#3103=EDGE_CURVE('',#2523,#2538,#2158,.T.);
#3104=EDGE_CURVE('',#2538,#2539,#2159,.T.);
#3105=EDGE_CURVE('',#2539,#2524,#2160,.T.);
#3106=EDGE_CURVE('',#2540,#2539,#27,.T.);
#3107=EDGE_CURVE('',#2525,#2540,#2161,.T.);
#3108=EDGE_CURVE('',#2541,#2541,#2162,.T.);
#3109=EDGE_CURVE('',#2541,#2534,#637,.T.);
#3110=EDGE_CURVE('',#2542,#2509,#2163,.T.);
#3111=EDGE_CURVE('',#2542,#2543,#28,.T.);
#3112=EDGE_CURVE('',#2540,#2543,#2164,.T.);
#3113=EDGE_CURVE('',#2527,#2542,#2165,.T.);
#3114=EDGE_CURVE('',#2543,#2526,#2166,.T.);
#3115=EDGE_CURVE('',#2544,#2544,#2167,.T.);
#3116=EDGE_CURVE('',#2545,#2545,#2168,.T.);
#3117=EDGE_CURVE('',#2546,#2546,#2169,.T.);
#3118=EDGE_CURVE('',#2546,#2544,#638,.T.);
#3119=EDGE_CURVE('',#2547,#2547,#2170,.T.);
#3120=EDGE_CURVE('',#2547,#2545,#639,.T.);
#3121=EDGE_CURVE('',#2548,#2548,#2171,.T.);
#3122=EDGE_CURVE('',#2549,#2549,#2172,.T.);
#3123=EDGE_CURVE('',#2550,#2550,#2173,.T.);
#3124=EDGE_CURVE('',#2550,#2548,#640,.T.);
#3125=EDGE_CURVE('',#2551,#2551,#2174,.T.);
#3126=EDGE_CURVE('',#2551,#2549,#641,.T.);
#3127=EDGE_CURVE('',#2552,#2553,#642,.T.);
#3128=EDGE_CURVE('',#2553,#2554,#643,.T.);
#3129=EDGE_CURVE('',#2554,#2555,#644,.T.);
#3130=EDGE_CURVE('',#2552,#2555,#645,.T.);
#3131=EDGE_CURVE('',#2553,#2556,#646,.T.);
#3132=EDGE_CURVE('',#2556,#2557,#647,.T.);
#3133=EDGE_CURVE('',#2557,#2554,#648,.T.);
#3134=EDGE_CURVE('',#2556,#2558,#649,.T.);
#3135=EDGE_CURVE('',#2558,#2559,#650,.T.);
#3136=EDGE_CURVE('',#2559,#2557,#651,.T.);
#3137=EDGE_CURVE('',#2558,#2560,#652,.T.);
#3138=EDGE_CURVE('',#2560,#2561,#653,.T.);
#3139=EDGE_CURVE('',#2561,#2559,#654,.T.);
#3140=EDGE_CURVE('',#2560,#2562,#655,.T.);
#3141=EDGE_CURVE('',#2562,#2563,#656,.T.);
#3142=EDGE_CURVE('',#2563,#2561,#657,.T.);
#3143=EDGE_CURVE('',#2562,#2552,#658,.T.);
#3144=EDGE_CURVE('',#2555,#2563,#659,.T.);
#3145=EDGE_CURVE('',#2564,#2564,#2175,.T.);
#3146=EDGE_CURVE('',#2565,#2565,#2176,.T.);
#3147=EDGE_CURVE('',#2566,#2566,#2177,.T.);
#3148=EDGE_CURVE('',#2566,#2565,#660,.T.);
#3149=EDGE_CURVE('',#2567,#2567,#2178,.T.);
#3150=EDGE_CURVE('',#2567,#2566,#661,.T.);
#3151=EDGE_CURVE('',#2568,#2568,#2179,.T.);
#3152=EDGE_CURVE('',#2568,#2567,#662,.T.);
#3153=EDGE_CURVE('',#2569,#2569,#2180,.T.);
#3154=EDGE_CURVE('',#2570,#2570,#2181,.F.);
#3155=EDGE_CURVE('',#2570,#2569,#663,.T.);
#3156=EDGE_CURVE('',#2564,#2570,#664,.T.);
#3157=EDGE_CURVE('',#2571,#2571,#2182,.T.);
#3158=EDGE_CURVE('',#2572,#2572,#2183,.T.);
#3159=EDGE_CURVE('',#2573,#2573,#2184,.T.);
#3160=EDGE_CURVE('',#2574,#2574,#2185,.T.);
#3161=EDGE_CURVE('',#2571,#2573,#665,.T.);
#3162=EDGE_CURVE('',#2574,#2575,#666,.T.);
#3163=EDGE_CURVE('',#2576,#2575,#2186,.T.);
#3164=EDGE_CURVE('',#2577,#2576,#2187,.T.);
#3165=EDGE_CURVE('',#2575,#2577,#2188,.T.);
#3166=EDGE_CURVE('',#2578,#2578,#2189,.T.);
#3167=EDGE_CURVE('',#2578,#2572,#667,.T.);
#3168=EDGE_CURVE('',#2579,#2576,#668,.T.);
#3169=EDGE_CURVE('',#2579,#2580,#669,.T.);
#3170=EDGE_CURVE('',#2577,#2580,#670,.T.);
#3171=EDGE_CURVE('',#2581,#2577,#671,.T.);
#3172=EDGE_CURVE('',#2582,#2581,#672,.T.);
#3173=EDGE_CURVE('',#2576,#2582,#673,.T.);
#3174=EDGE_CURVE('',#2583,#2584,#674,.T.);
#3175=EDGE_CURVE('',#2582,#2583,#675,.T.);
#3176=EDGE_CURVE('',#2584,#2581,#676,.T.);
#3177=EDGE_CURVE('',#2585,#2586,#677,.T.);
#3178=EDGE_CURVE('',#2587,#2585,#678,.T.);
#3179=EDGE_CURVE('',#2588,#2587,#679,.T.);
#3180=EDGE_CURVE('',#2586,#2588,#680,.T.);
#3181=EDGE_CURVE('',#2580,#2587,#681,.T.);
#3182=EDGE_CURVE('',#2585,#2589,#2190,.T.);
#3183=EDGE_CURVE('',#2589,#2590,#682,.T.);
#3184=EDGE_CURVE('',#2590,#2584,#2191,.T.);
#3185=EDGE_CURVE('',#2586,#2591,#2192,.T.);
#3186=EDGE_CURVE('',#2591,#2589,#683,.T.);
#3187=EDGE_CURVE('',#2588,#2579,#684,.T.);
#3188=EDGE_CURVE('',#2592,#2583,#2193,.T.);
#3189=EDGE_CURVE('',#2592,#2591,#685,.T.);
#3190=EDGE_CURVE('',#2590,#2592,#686,.T.);
#3191=EDGE_CURVE('',#2593,#2593,#2194,.T.);
#3192=EDGE_CURVE('',#2593,#2594,#687,.T.);
#3193=EDGE_CURVE('',#2594,#2594,#2195,.T.);
#3194=EDGE_CURVE('',#2595,#2595,#2196,.T.);
#3195=EDGE_CURVE('',#2595,#2596,#688,.T.);
#3196=EDGE_CURVE('',#2596,#2596,#2197,.T.);
#3197=EDGE_CURVE('',#2597,#2597,#2198,.T.);
#3198=EDGE_CURVE('',#2597,#2598,#689,.T.);
#3199=EDGE_CURVE('',#2598,#2598,#2199,.T.);
#3200=EDGE_CURVE('',#2599,#2600,#690,.T.);
#3201=EDGE_CURVE('',#2600,#2601,#691,.T.);
#3202=EDGE_CURVE('',#2602,#2601,#692,.T.);
#3203=EDGE_CURVE('',#2599,#2602,#693,.T.);
#3204=EDGE_CURVE('',#2603,#2599,#694,.T.);
#3205=EDGE_CURVE('',#2604,#2602,#695,.T.);
#3206=EDGE_CURVE('',#2603,#2604,#696,.T.);
#3207=EDGE_CURVE('',#2605,#2603,#697,.T.);
#3208=EDGE_CURVE('',#2606,#2604,#698,.T.);
#3209=EDGE_CURVE('',#2605,#2606,#699,.T.);
#3210=EDGE_CURVE('',#2607,#2605,#700,.T.);
#3211=EDGE_CURVE('',#2608,#2606,#701,.T.);
#3212=EDGE_CURVE('',#2607,#2608,#702,.T.);
#3213=EDGE_CURVE('',#2609,#2607,#703,.T.);
#3214=EDGE_CURVE('',#2610,#2608,#704,.T.);
#3215=EDGE_CURVE('',#2609,#2610,#705,.T.);
#3216=EDGE_CURVE('',#2600,#2609,#706,.T.);
#3217=EDGE_CURVE('',#2601,#2610,#707,.T.);
#3218=EDGE_CURVE('',#2611,#2611,#2200,.T.);
#3219=EDGE_CURVE('',#2611,#2612,#708,.T.);
#3220=EDGE_CURVE('',#2612,#2612,#2201,.T.);
#3221=EDGE_CURVE('',#2613,#2613,#2202,.T.);
#3222=EDGE_CURVE('',#2613,#2614,#709,.T.);
#3223=EDGE_CURVE('',#2614,#2614,#2203,.T.);
#3224=EDGE_CURVE('',#2615,#2616,#710,.T.);
#3225=EDGE_CURVE('',#2615,#2617,#2204,.T.);
#3226=EDGE_CURVE('',#2618,#2617,#711,.T.);
#3227=EDGE_CURVE('',#2616,#2618,#2205,.T.);
#3228=EDGE_CURVE('',#2618,#2616,#2206,.T.);
#3229=EDGE_CURVE('',#2617,#2615,#2207,.T.);
#3230=ORIENTED_EDGE('',*,*,#2619,.F.);
#3231=ORIENTED_EDGE('',*,*,#2620,.T.);
#3232=ORIENTED_EDGE('',*,*,#2621,.F.);
#3233=ORIENTED_EDGE('',*,*,#2622,.T.);
#3234=ORIENTED_EDGE('',*,*,#2623,.F.);
#3235=ORIENTED_EDGE('',*,*,#2624,.T.);
#3236=ORIENTED_EDGE('',*,*,#2625,.F.);
#3237=ORIENTED_EDGE('',*,*,#2626,.T.);
#3238=ORIENTED_EDGE('',*,*,#2627,.T.);
#3239=ORIENTED_EDGE('',*,*,#2628,.F.);
#3240=ORIENTED_EDGE('',*,*,#2624,.F.);
#3241=ORIENTED_EDGE('',*,*,#2629,.F.);
#3242=ORIENTED_EDGE('',*,*,#2630,.F.);
#3243=ORIENTED_EDGE('',*,*,#2631,.F.);
#3244=ORIENTED_EDGE('',*,*,#2632,.F.);
#3245=ORIENTED_EDGE('',*,*,#2633,.F.);
#3246=ORIENTED_EDGE('',*,*,#2622,.F.);
#3247=ORIENTED_EDGE('',*,*,#2634,.F.);
#3248=ORIENTED_EDGE('',*,*,#2626,.F.);
#3249=ORIENTED_EDGE('',*,*,#2635,.F.);
#3250=ORIENTED_EDGE('',*,*,#2636,.F.);
#3251=ORIENTED_EDGE('',*,*,#2627,.F.);
#3252=ORIENTED_EDGE('',*,*,#2637,.T.);
#3253=ORIENTED_EDGE('',*,*,#2638,.F.);
#3254=ORIENTED_EDGE('',*,*,#2637,.F.);
#3255=ORIENTED_EDGE('',*,*,#2639,.F.);
#3256=ORIENTED_EDGE('',*,*,#2640,.F.);
#3257=ORIENTED_EDGE('',*,*,#2641,.F.);
#3258=ORIENTED_EDGE('',*,*,#2620,.F.);
#3259=ORIENTED_EDGE('',*,*,#2642,.F.);
#3260=ORIENTED_EDGE('',*,*,#2643,.T.);
#3261=ORIENTED_EDGE('',*,*,#2644,.F.);
#3262=ORIENTED_EDGE('',*,*,#2639,.T.);
#3263=ORIENTED_EDGE('',*,*,#2619,.T.);
#3264=ORIENTED_EDGE('',*,*,#2634,.T.);
#3265=ORIENTED_EDGE('',*,*,#2645,.F.);
#3266=ORIENTED_EDGE('',*,*,#2643,.F.);
#3267=ORIENTED_EDGE('',*,*,#2646,.F.);
#3268=ORIENTED_EDGE('',*,*,#2647,.T.);
#3269=ORIENTED_EDGE('',*,*,#2648,.F.);
#3270=ORIENTED_EDGE('',*,*,#2635,.T.);
#3271=ORIENTED_EDGE('',*,*,#2625,.T.);
#3272=ORIENTED_EDGE('',*,*,#2628,.T.);
#3273=ORIENTED_EDGE('',*,*,#2649,.F.);
#3274=ORIENTED_EDGE('',*,*,#2647,.F.);
#3275=ORIENTED_EDGE('',*,*,#2650,.F.);
#3276=ORIENTED_EDGE('',*,*,#2651,.T.);
#3277=ORIENTED_EDGE('',*,*,#2652,.F.);
#3278=ORIENTED_EDGE('',*,*,#2629,.T.);
#3279=ORIENTED_EDGE('',*,*,#2623,.T.);
#3280=ORIENTED_EDGE('',*,*,#2633,.T.);
#3281=ORIENTED_EDGE('',*,*,#2653,.F.);
#3282=ORIENTED_EDGE('',*,*,#2651,.F.);
#3283=ORIENTED_EDGE('',*,*,#2638,.T.);
#3284=ORIENTED_EDGE('',*,*,#2654,.T.);
#3285=ORIENTED_EDGE('',*,*,#2655,.F.);
#3286=ORIENTED_EDGE('',*,*,#2656,.T.);
#3287=ORIENTED_EDGE('',*,*,#2657,.F.);
#3288=ORIENTED_EDGE('',*,*,#2631,.T.);
#3289=ORIENTED_EDGE('',*,*,#2621,.T.);
#3290=ORIENTED_EDGE('',*,*,#2641,.T.);
#3291=ORIENTED_EDGE('',*,*,#2658,.F.);
#3292=ORIENTED_EDGE('',*,*,#2656,.F.);
#3293=ORIENTED_EDGE('',*,*,#2659,.F.);
#3294=ORIENTED_EDGE('',*,*,#2660,.T.);
#3295=ORIENTED_EDGE('',*,*,#2661,.F.);
#3296=ORIENTED_EDGE('',*,*,#2660,.F.);
#3297=ORIENTED_EDGE('',*,*,#2662,.F.);
#3298=ORIENTED_EDGE('',*,*,#2663,.T.);
#3299=ORIENTED_EDGE('',*,*,#2664,.F.);
#3300=ORIENTED_EDGE('',*,*,#2663,.F.);
#3301=ORIENTED_EDGE('',*,*,#2665,.F.);
#3302=ORIENTED_EDGE('',*,*,#2666,.T.);
#3303=ORIENTED_EDGE('',*,*,#2667,.F.);
#3304=ORIENTED_EDGE('',*,*,#2666,.F.);
#3305=ORIENTED_EDGE('',*,*,#2668,.F.);
#3306=ORIENTED_EDGE('',*,*,#2669,.T.);
#3307=ORIENTED_EDGE('',*,*,#2654,.F.);
#3308=ORIENTED_EDGE('',*,*,#2669,.F.);
#3309=ORIENTED_EDGE('',*,*,#2670,.F.);
#3310=ORIENTED_EDGE('',*,*,#2671,.T.);
#3311=ORIENTED_EDGE('',*,*,#2672,.F.);
#3312=ORIENTED_EDGE('',*,*,#2673,.F.);
#3313=ORIENTED_EDGE('',*,*,#2674,.F.);
#3314=ORIENTED_EDGE('',*,*,#2673,.T.);
#3315=ORIENTED_EDGE('',*,*,#2675,.F.);
#3316=ORIENTED_EDGE('',*,*,#2676,.F.);
#3317=ORIENTED_EDGE('',*,*,#2677,.F.);
#3318=ORIENTED_EDGE('',*,*,#2676,.T.);
#3319=ORIENTED_EDGE('',*,*,#2678,.F.);
#3320=ORIENTED_EDGE('',*,*,#2679,.F.);
#3321=ORIENTED_EDGE('',*,*,#2680,.F.);
#3322=ORIENTED_EDGE('',*,*,#2679,.T.);
#3323=ORIENTED_EDGE('',*,*,#2681,.F.);
#3324=ORIENTED_EDGE('',*,*,#2682,.F.);
#3325=ORIENTED_EDGE('',*,*,#2683,.F.);
#3326=ORIENTED_EDGE('',*,*,#2682,.T.);
#3327=ORIENTED_EDGE('',*,*,#2684,.F.);
#3328=ORIENTED_EDGE('',*,*,#2685,.F.);
#3329=ORIENTED_EDGE('',*,*,#2686,.F.);
#3330=ORIENTED_EDGE('',*,*,#2685,.T.);
#3331=ORIENTED_EDGE('',*,*,#2687,.F.);
#3332=ORIENTED_EDGE('',*,*,#2688,.F.);
#3333=ORIENTED_EDGE('',*,*,#2689,.F.);
#3334=ORIENTED_EDGE('',*,*,#2688,.T.);
#3335=ORIENTED_EDGE('',*,*,#2690,.F.);
#3336=ORIENTED_EDGE('',*,*,#2691,.F.);
#3337=ORIENTED_EDGE('',*,*,#2692,.F.);
#3338=ORIENTED_EDGE('',*,*,#2691,.T.);
#3339=ORIENTED_EDGE('',*,*,#2693,.F.);
#3340=ORIENTED_EDGE('',*,*,#2671,.F.);
#3341=ORIENTED_EDGE('',*,*,#2693,.T.);
#3342=ORIENTED_EDGE('',*,*,#2690,.T.);
#3343=ORIENTED_EDGE('',*,*,#2687,.T.);
#3344=ORIENTED_EDGE('',*,*,#2684,.T.);
#3345=ORIENTED_EDGE('',*,*,#2681,.T.);
#3346=ORIENTED_EDGE('',*,*,#2678,.T.);
#3347=ORIENTED_EDGE('',*,*,#2675,.T.);
#3348=ORIENTED_EDGE('',*,*,#2672,.T.);
#3349=ORIENTED_EDGE('',*,*,#2640,.T.);
#3350=ORIENTED_EDGE('',*,*,#2644,.T.);
#3351=ORIENTED_EDGE('',*,*,#2645,.T.);
#3352=ORIENTED_EDGE('',*,*,#2636,.T.);
#3353=ORIENTED_EDGE('',*,*,#2648,.T.);
#3354=ORIENTED_EDGE('',*,*,#2649,.T.);
#3355=ORIENTED_EDGE('',*,*,#2630,.T.);
#3356=ORIENTED_EDGE('',*,*,#2652,.T.);
#3357=ORIENTED_EDGE('',*,*,#2653,.T.);
#3358=ORIENTED_EDGE('',*,*,#2632,.T.);
#3359=ORIENTED_EDGE('',*,*,#2657,.T.);
#3360=ORIENTED_EDGE('',*,*,#2658,.T.);
#3361=ORIENTED_EDGE('',*,*,#2667,.T.);
#3362=ORIENTED_EDGE('',*,*,#2664,.T.);
#3363=ORIENTED_EDGE('',*,*,#2661,.T.);
#3364=ORIENTED_EDGE('',*,*,#2692,.T.);
#3365=ORIENTED_EDGE('',*,*,#2670,.T.);
#3366=ORIENTED_EDGE('',*,*,#2674,.T.);
#3367=ORIENTED_EDGE('',*,*,#2677,.T.);
#3368=ORIENTED_EDGE('',*,*,#2680,.T.);
#3369=ORIENTED_EDGE('',*,*,#2683,.T.);
#3370=ORIENTED_EDGE('',*,*,#2686,.T.);
#3371=ORIENTED_EDGE('',*,*,#2689,.T.);
#3372=ORIENTED_EDGE('',*,*,#2668,.T.);
#3373=ORIENTED_EDGE('',*,*,#2665,.T.);
#3374=ORIENTED_EDGE('',*,*,#2662,.T.);
#3375=ORIENTED_EDGE('',*,*,#2659,.T.);
#3376=ORIENTED_EDGE('',*,*,#2650,.T.);
#3377=ORIENTED_EDGE('',*,*,#2642,.T.);
#3378=ORIENTED_EDGE('',*,*,#2655,.T.);
#3379=ORIENTED_EDGE('',*,*,#2646,.T.);
#3380=ORIENTED_EDGE('',*,*,#2694,.F.);
#3381=ORIENTED_EDGE('',*,*,#2695,.F.);
#3382=ORIENTED_EDGE('',*,*,#2696,.F.);
#3383=ORIENTED_EDGE('',*,*,#2697,.F.);
#3384=ORIENTED_EDGE('',*,*,#2698,.F.);
#3385=ORIENTED_EDGE('',*,*,#2699,.F.);
#3386=ORIENTED_EDGE('',*,*,#2700,.F.);
#3387=ORIENTED_EDGE('',*,*,#2701,.F.);
#3388=ORIENTED_EDGE('',*,*,#2702,.F.);
#3389=ORIENTED_EDGE('',*,*,#2703,.F.);
#3390=ORIENTED_EDGE('',*,*,#2699,.T.);
#3391=ORIENTED_EDGE('',*,*,#2704,.F.);
#3392=ORIENTED_EDGE('',*,*,#2705,.F.);
#3393=ORIENTED_EDGE('',*,*,#2706,.F.);
#3394=ORIENTED_EDGE('',*,*,#2701,.T.);
#3395=ORIENTED_EDGE('',*,*,#2707,.F.);
#3396=ORIENTED_EDGE('',*,*,#2708,.F.);
#3397=ORIENTED_EDGE('',*,*,#2709,.F.);
#3398=ORIENTED_EDGE('',*,*,#2710,.F.);
#3399=ORIENTED_EDGE('',*,*,#2711,.F.);
#3400=ORIENTED_EDGE('',*,*,#2697,.T.);
#3401=ORIENTED_EDGE('',*,*,#2712,.F.);
#3402=ORIENTED_EDGE('',*,*,#2713,.T.);
#3403=ORIENTED_EDGE('',*,*,#2702,.T.);
#3404=ORIENTED_EDGE('',*,*,#2713,.F.);
#3405=ORIENTED_EDGE('',*,*,#2714,.F.);
#3406=ORIENTED_EDGE('',*,*,#2715,.F.);
#3407=ORIENTED_EDGE('',*,*,#2716,.F.);
#3408=ORIENTED_EDGE('',*,*,#2695,.T.);
#3409=ORIENTED_EDGE('',*,*,#2714,.T.);
#3410=ORIENTED_EDGE('',*,*,#2694,.T.);
#3411=ORIENTED_EDGE('',*,*,#2706,.T.);
#3412=ORIENTED_EDGE('',*,*,#2717,.F.);
#3413=ORIENTED_EDGE('',*,*,#2718,.T.);
#3414=ORIENTED_EDGE('',*,*,#2719,.F.);
#3415=ORIENTED_EDGE('',*,*,#2718,.F.);
#3416=ORIENTED_EDGE('',*,*,#2720,.F.);
#3417=ORIENTED_EDGE('',*,*,#2707,.T.);
#3418=ORIENTED_EDGE('',*,*,#2700,.T.);
#3419=ORIENTED_EDGE('',*,*,#2703,.T.);
#3420=ORIENTED_EDGE('',*,*,#2721,.F.);
#3421=ORIENTED_EDGE('',*,*,#2722,.T.);
#3422=ORIENTED_EDGE('',*,*,#2723,.F.);
#3423=ORIENTED_EDGE('',*,*,#2722,.F.);
#3424=ORIENTED_EDGE('',*,*,#2724,.F.);
#3425=ORIENTED_EDGE('',*,*,#2712,.T.);
#3426=ORIENTED_EDGE('',*,*,#2725,.T.);
#3427=ORIENTED_EDGE('',*,*,#2716,.T.);
#3428=ORIENTED_EDGE('',*,*,#2726,.F.);
#3429=ORIENTED_EDGE('',*,*,#2727,.T.);
#3430=ORIENTED_EDGE('',*,*,#2728,.F.);
#3431=ORIENTED_EDGE('',*,*,#2727,.F.);
#3432=ORIENTED_EDGE('',*,*,#2729,.F.);
#3433=ORIENTED_EDGE('',*,*,#2709,.T.);
#3434=ORIENTED_EDGE('',*,*,#2696,.T.);
#3435=ORIENTED_EDGE('',*,*,#2711,.T.);
#3436=ORIENTED_EDGE('',*,*,#2730,.F.);
#3437=ORIENTED_EDGE('',*,*,#2731,.T.);
#3438=ORIENTED_EDGE('',*,*,#2732,.F.);
#3439=ORIENTED_EDGE('',*,*,#2731,.F.);
#3440=ORIENTED_EDGE('',*,*,#2733,.F.);
#3441=ORIENTED_EDGE('',*,*,#2704,.T.);
#3442=ORIENTED_EDGE('',*,*,#2698,.T.);
#3443=ORIENTED_EDGE('',*,*,#2734,.F.);
#3444=ORIENTED_EDGE('',*,*,#2735,.T.);
#3445=ORIENTED_EDGE('',*,*,#2736,.F.);
#3446=ORIENTED_EDGE('',*,*,#2735,.F.);
#3447=ORIENTED_EDGE('',*,*,#2737,.F.);
#3448=ORIENTED_EDGE('',*,*,#2738,.T.);
#3449=ORIENTED_EDGE('',*,*,#2739,.F.);
#3450=ORIENTED_EDGE('',*,*,#2738,.F.);
#3451=ORIENTED_EDGE('',*,*,#2740,.F.);
#3452=ORIENTED_EDGE('',*,*,#2741,.T.);
#3453=ORIENTED_EDGE('',*,*,#2742,.F.);
#3454=ORIENTED_EDGE('',*,*,#2741,.F.);
#3455=ORIENTED_EDGE('',*,*,#2725,.F.);
#3456=ORIENTED_EDGE('',*,*,#2743,.T.);
#3457=ORIENTED_EDGE('',*,*,#2744,.F.);
#3458=ORIENTED_EDGE('',*,*,#2743,.F.);
#3459=ORIENTED_EDGE('',*,*,#2745,.F.);
#3460=ORIENTED_EDGE('',*,*,#2746,.T.);
#3461=ORIENTED_EDGE('',*,*,#2747,.F.);
#3462=ORIENTED_EDGE('',*,*,#2748,.F.);
#3463=ORIENTED_EDGE('',*,*,#2749,.F.);
#3464=ORIENTED_EDGE('',*,*,#2748,.T.);
#3465=ORIENTED_EDGE('',*,*,#2750,.F.);
#3466=ORIENTED_EDGE('',*,*,#2751,.F.);
#3467=ORIENTED_EDGE('',*,*,#2752,.F.);
#3468=ORIENTED_EDGE('',*,*,#2751,.T.);
#3469=ORIENTED_EDGE('',*,*,#2753,.F.);
#3470=ORIENTED_EDGE('',*,*,#2754,.F.);
#3471=ORIENTED_EDGE('',*,*,#2755,.F.);
#3472=ORIENTED_EDGE('',*,*,#2754,.T.);
#3473=ORIENTED_EDGE('',*,*,#2756,.F.);
#3474=ORIENTED_EDGE('',*,*,#2757,.F.);
#3475=ORIENTED_EDGE('',*,*,#2758,.F.);
#3476=ORIENTED_EDGE('',*,*,#2757,.T.);
#3477=ORIENTED_EDGE('',*,*,#2759,.F.);
#3478=ORIENTED_EDGE('',*,*,#2760,.F.);
#3479=ORIENTED_EDGE('',*,*,#2761,.F.);
#3480=ORIENTED_EDGE('',*,*,#2760,.T.);
#3481=ORIENTED_EDGE('',*,*,#2762,.F.);
#3482=ORIENTED_EDGE('',*,*,#2763,.F.);
#3483=ORIENTED_EDGE('',*,*,#2764,.F.);
#3484=ORIENTED_EDGE('',*,*,#2763,.T.);
#3485=ORIENTED_EDGE('',*,*,#2765,.F.);
#3486=ORIENTED_EDGE('',*,*,#2766,.F.);
#3487=ORIENTED_EDGE('',*,*,#2767,.F.);
#3488=ORIENTED_EDGE('',*,*,#2766,.T.);
#3489=ORIENTED_EDGE('',*,*,#2768,.F.);
#3490=ORIENTED_EDGE('',*,*,#2746,.F.);
#3491=ORIENTED_EDGE('',*,*,#2768,.T.);
#3492=ORIENTED_EDGE('',*,*,#2765,.T.);
#3493=ORIENTED_EDGE('',*,*,#2762,.T.);
#3494=ORIENTED_EDGE('',*,*,#2759,.T.);
#3495=ORIENTED_EDGE('',*,*,#2756,.T.);
#3496=ORIENTED_EDGE('',*,*,#2753,.T.);
#3497=ORIENTED_EDGE('',*,*,#2750,.T.);
#3498=ORIENTED_EDGE('',*,*,#2747,.T.);
#3499=ORIENTED_EDGE('',*,*,#2744,.T.);
#3500=ORIENTED_EDGE('',*,*,#2742,.T.);
#3501=ORIENTED_EDGE('',*,*,#2739,.T.);
#3502=ORIENTED_EDGE('',*,*,#2736,.T.);
#3503=ORIENTED_EDGE('',*,*,#2732,.T.);
#3504=ORIENTED_EDGE('',*,*,#2719,.T.);
#3505=ORIENTED_EDGE('',*,*,#2723,.T.);
#3506=ORIENTED_EDGE('',*,*,#2728,.T.);
#3507=ORIENTED_EDGE('',*,*,#2767,.T.);
#3508=ORIENTED_EDGE('',*,*,#2745,.T.);
#3509=ORIENTED_EDGE('',*,*,#2749,.T.);
#3510=ORIENTED_EDGE('',*,*,#2752,.T.);
#3511=ORIENTED_EDGE('',*,*,#2755,.T.);
#3512=ORIENTED_EDGE('',*,*,#2758,.T.);
#3513=ORIENTED_EDGE('',*,*,#2761,.T.);
#3514=ORIENTED_EDGE('',*,*,#2764,.T.);
#3515=ORIENTED_EDGE('',*,*,#2715,.T.);
#3516=ORIENTED_EDGE('',*,*,#2720,.T.);
#3517=ORIENTED_EDGE('',*,*,#2717,.T.);
#3518=ORIENTED_EDGE('',*,*,#2708,.T.);
#3519=ORIENTED_EDGE('',*,*,#2724,.T.);
#3520=ORIENTED_EDGE('',*,*,#2721,.T.);
#3521=ORIENTED_EDGE('',*,*,#2705,.T.);
#3522=ORIENTED_EDGE('',*,*,#2733,.T.);
#3523=ORIENTED_EDGE('',*,*,#2730,.T.);
#3524=ORIENTED_EDGE('',*,*,#2710,.T.);
#3525=ORIENTED_EDGE('',*,*,#2729,.T.);
#3526=ORIENTED_EDGE('',*,*,#2726,.T.);
#3527=ORIENTED_EDGE('',*,*,#2740,.T.);
#3528=ORIENTED_EDGE('',*,*,#2737,.T.);
#3529=ORIENTED_EDGE('',*,*,#2734,.T.);
#3530=ORIENTED_EDGE('',*,*,#2769,.F.);
#3531=ORIENTED_EDGE('',*,*,#2770,.T.);
#3532=ORIENTED_EDGE('',*,*,#2771,.F.);
#3533=ORIENTED_EDGE('',*,*,#2770,.F.);
#3534=ORIENTED_EDGE('',*,*,#2772,.F.);
#3535=ORIENTED_EDGE('',*,*,#2773,.T.);
#3536=ORIENTED_EDGE('',*,*,#2774,.F.);
#3537=ORIENTED_EDGE('',*,*,#2773,.F.);
#3538=ORIENTED_EDGE('',*,*,#2775,.F.);
#3539=ORIENTED_EDGE('',*,*,#2776,.T.);
#3540=ORIENTED_EDGE('',*,*,#2777,.F.);
#3541=ORIENTED_EDGE('',*,*,#2776,.F.);
#3542=ORIENTED_EDGE('',*,*,#2778,.T.);
#3543=ORIENTED_EDGE('',*,*,#2779,.T.);
#3544=ORIENTED_EDGE('',*,*,#2780,.F.);
#3545=ORIENTED_EDGE('',*,*,#2781,.F.);
#3546=ORIENTED_EDGE('',*,*,#2774,.T.);
#3547=ORIENTED_EDGE('',*,*,#2777,.T.);
#3548=ORIENTED_EDGE('',*,*,#2782,.T.);
#3549=ORIENTED_EDGE('',*,*,#2781,.T.);
#3550=ORIENTED_EDGE('',*,*,#2783,.F.);
#3551=ORIENTED_EDGE('',*,*,#2784,.F.);
#3552=ORIENTED_EDGE('',*,*,#2785,.T.);
#3553=ORIENTED_EDGE('',*,*,#2784,.T.);
#3554=ORIENTED_EDGE('',*,*,#2786,.F.);
#3555=ORIENTED_EDGE('',*,*,#2787,.F.);
#3556=ORIENTED_EDGE('',*,*,#2772,.T.);
#3557=ORIENTED_EDGE('',*,*,#2775,.T.);
#3558=ORIENTED_EDGE('',*,*,#2788,.T.);
#3559=ORIENTED_EDGE('',*,*,#2787,.T.);
#3560=ORIENTED_EDGE('',*,*,#2789,.F.);
#3561=ORIENTED_EDGE('',*,*,#2779,.F.);
#3562=ORIENTED_EDGE('',*,*,#2789,.T.);
#3563=ORIENTED_EDGE('',*,*,#2786,.T.);
#3564=ORIENTED_EDGE('',*,*,#2783,.T.);
#3565=ORIENTED_EDGE('',*,*,#2780,.T.);
#3566=ORIENTED_EDGE('',*,*,#2771,.T.);
#3567=ORIENTED_EDGE('',*,*,#2788,.F.);
#3568=ORIENTED_EDGE('',*,*,#2778,.F.);
#3569=ORIENTED_EDGE('',*,*,#2782,.F.);
#3570=ORIENTED_EDGE('',*,*,#2785,.F.);
#3571=ORIENTED_EDGE('',*,*,#2769,.T.);
#3572=ORIENTED_EDGE('',*,*,#2790,.F.);
#3573=ORIENTED_EDGE('',*,*,#2791,.T.);
#3574=ORIENTED_EDGE('',*,*,#2792,.T.);
#3575=ORIENTED_EDGE('',*,*,#2791,.F.);
#3576=ORIENTED_EDGE('',*,*,#2793,.F.);
#3577=ORIENTED_EDGE('',*,*,#2794,.T.);
#3578=ORIENTED_EDGE('',*,*,#2795,.T.);
#3579=ORIENTED_EDGE('',*,*,#2794,.F.);
#3580=ORIENTED_EDGE('',*,*,#2793,.T.);
#3581=ORIENTED_EDGE('',*,*,#2790,.T.);
#3582=ORIENTED_EDGE('',*,*,#2795,.F.);
#3583=ORIENTED_EDGE('',*,*,#2792,.F.);
#3584=ORIENTED_EDGE('',*,*,#2796,.F.);
#3585=ORIENTED_EDGE('',*,*,#2797,.T.);
#3586=ORIENTED_EDGE('',*,*,#2798,.F.);
#3587=ORIENTED_EDGE('',*,*,#2797,.F.);
#3588=ORIENTED_EDGE('',*,*,#2796,.T.);
#3589=ORIENTED_EDGE('',*,*,#2799,.T.);
#3590=ORIENTED_EDGE('',*,*,#2800,.F.);
#3591=ORIENTED_EDGE('',*,*,#2799,.F.);
#3592=ORIENTED_EDGE('',*,*,#2801,.T.);
#3593=ORIENTED_EDGE('',*,*,#2802,.T.);
#3594=ORIENTED_EDGE('',*,*,#2801,.F.);
#3595=ORIENTED_EDGE('',*,*,#2802,.F.);
#3596=ORIENTED_EDGE('',*,*,#2803,.F.);
#3597=ORIENTED_EDGE('',*,*,#2804,.T.);
#3598=ORIENTED_EDGE('',*,*,#2800,.T.);
#3599=ORIENTED_EDGE('',*,*,#2804,.F.);
#3600=ORIENTED_EDGE('',*,*,#2803,.T.);
#3601=ORIENTED_EDGE('',*,*,#2798,.T.);
#3602=ORIENTED_EDGE('',*,*,#2805,.F.);
#3603=ORIENTED_EDGE('',*,*,#2806,.T.);
#3604=ORIENTED_EDGE('',*,*,#2807,.T.);
#3605=ORIENTED_EDGE('',*,*,#2806,.F.);
#3606=ORIENTED_EDGE('',*,*,#2808,.F.);
#3607=ORIENTED_EDGE('',*,*,#2809,.T.);
#3608=ORIENTED_EDGE('',*,*,#2810,.T.);
#3609=ORIENTED_EDGE('',*,*,#2809,.F.);
#3610=ORIENTED_EDGE('',*,*,#2808,.T.);
#3611=ORIENTED_EDGE('',*,*,#2805,.T.);
#3612=ORIENTED_EDGE('',*,*,#2810,.F.);
#3613=ORIENTED_EDGE('',*,*,#2807,.F.);
#3614=ORIENTED_EDGE('',*,*,#2811,.F.);
#3615=ORIENTED_EDGE('',*,*,#2812,.T.);
#3616=ORIENTED_EDGE('',*,*,#2813,.T.);
#3617=ORIENTED_EDGE('',*,*,#2812,.F.);
#3618=ORIENTED_EDGE('',*,*,#2814,.F.);
#3619=ORIENTED_EDGE('',*,*,#2815,.T.);
#3620=ORIENTED_EDGE('',*,*,#2816,.T.);
#3621=ORIENTED_EDGE('',*,*,#2815,.F.);
#3622=ORIENTED_EDGE('',*,*,#2814,.T.);
#3623=ORIENTED_EDGE('',*,*,#2811,.T.);
#3624=ORIENTED_EDGE('',*,*,#2816,.F.);
#3625=ORIENTED_EDGE('',*,*,#2813,.F.);
#3626=ORIENTED_EDGE('',*,*,#2817,.F.);
#3627=ORIENTED_EDGE('',*,*,#2818,.T.);
#3628=ORIENTED_EDGE('',*,*,#2819,.T.);
#3629=ORIENTED_EDGE('',*,*,#2818,.F.);
#3630=ORIENTED_EDGE('',*,*,#2820,.F.);
#3631=ORIENTED_EDGE('',*,*,#2821,.T.);
#3632=ORIENTED_EDGE('',*,*,#2822,.T.);
#3633=ORIENTED_EDGE('',*,*,#2821,.F.);
#3634=ORIENTED_EDGE('',*,*,#2820,.T.);
#3635=ORIENTED_EDGE('',*,*,#2817,.T.);
#3636=ORIENTED_EDGE('',*,*,#2822,.F.);
#3637=ORIENTED_EDGE('',*,*,#2819,.F.);
#3638=ORIENTED_EDGE('',*,*,#2823,.F.);
#3639=ORIENTED_EDGE('',*,*,#2824,.T.);
#3640=ORIENTED_EDGE('',*,*,#2825,.T.);
#3641=ORIENTED_EDGE('',*,*,#2824,.F.);
#3642=ORIENTED_EDGE('',*,*,#2826,.F.);
#3643=ORIENTED_EDGE('',*,*,#2827,.T.);
#3644=ORIENTED_EDGE('',*,*,#2828,.T.);
#3645=ORIENTED_EDGE('',*,*,#2827,.F.);
#3646=ORIENTED_EDGE('',*,*,#2826,.T.);
#3647=ORIENTED_EDGE('',*,*,#2823,.T.);
#3648=ORIENTED_EDGE('',*,*,#2828,.F.);
#3649=ORIENTED_EDGE('',*,*,#2825,.F.);
#3650=ORIENTED_EDGE('',*,*,#2829,.F.);
#3651=ORIENTED_EDGE('',*,*,#2830,.T.);
#3652=ORIENTED_EDGE('',*,*,#2831,.T.);
#3653=ORIENTED_EDGE('',*,*,#2830,.F.);
#3654=ORIENTED_EDGE('',*,*,#2832,.F.);
#3655=ORIENTED_EDGE('',*,*,#2833,.T.);
#3656=ORIENTED_EDGE('',*,*,#2834,.T.);
#3657=ORIENTED_EDGE('',*,*,#2833,.F.);
#3658=ORIENTED_EDGE('',*,*,#2832,.T.);
#3659=ORIENTED_EDGE('',*,*,#2829,.T.);
#3660=ORIENTED_EDGE('',*,*,#2834,.F.);
#3661=ORIENTED_EDGE('',*,*,#2831,.F.);
#3662=ORIENTED_EDGE('',*,*,#2835,.F.);
#3663=ORIENTED_EDGE('',*,*,#2836,.T.);
#3664=ORIENTED_EDGE('',*,*,#2837,.T.);
#3665=ORIENTED_EDGE('',*,*,#2836,.F.);
#3666=ORIENTED_EDGE('',*,*,#2838,.F.);
#3667=ORIENTED_EDGE('',*,*,#2839,.T.);
#3668=ORIENTED_EDGE('',*,*,#2840,.T.);
#3669=ORIENTED_EDGE('',*,*,#2839,.F.);
#3670=ORIENTED_EDGE('',*,*,#2838,.T.);
#3671=ORIENTED_EDGE('',*,*,#2835,.T.);
#3672=ORIENTED_EDGE('',*,*,#2840,.F.);
#3673=ORIENTED_EDGE('',*,*,#2837,.F.);
#3674=ORIENTED_EDGE('',*,*,#2841,.F.);
#3675=ORIENTED_EDGE('',*,*,#2842,.T.);
#3676=ORIENTED_EDGE('',*,*,#2843,.T.);
#3677=ORIENTED_EDGE('',*,*,#2842,.F.);
#3678=ORIENTED_EDGE('',*,*,#2844,.F.);
#3679=ORIENTED_EDGE('',*,*,#2845,.T.);
#3680=ORIENTED_EDGE('',*,*,#2846,.T.);
#3681=ORIENTED_EDGE('',*,*,#2845,.F.);
#3682=ORIENTED_EDGE('',*,*,#2844,.T.);
#3683=ORIENTED_EDGE('',*,*,#2841,.T.);
#3684=ORIENTED_EDGE('',*,*,#2846,.F.);
#3685=ORIENTED_EDGE('',*,*,#2843,.F.);
#3686=ORIENTED_EDGE('',*,*,#2847,.T.);
#3687=ORIENTED_EDGE('',*,*,#2848,.T.);
#3688=ORIENTED_EDGE('',*,*,#2849,.T.);
#3689=ORIENTED_EDGE('',*,*,#2850,.F.);
#3690=ORIENTED_EDGE('',*,*,#2851,.T.);
#3691=ORIENTED_EDGE('',*,*,#2852,.T.);
#3692=ORIENTED_EDGE('',*,*,#2853,.T.);
#3693=ORIENTED_EDGE('',*,*,#2848,.F.);
#3694=ORIENTED_EDGE('',*,*,#2854,.T.);
#3695=ORIENTED_EDGE('',*,*,#2855,.T.);
#3696=ORIENTED_EDGE('',*,*,#2856,.T.);
#3697=ORIENTED_EDGE('',*,*,#2852,.F.);
#3698=ORIENTED_EDGE('',*,*,#2857,.T.);
#3699=ORIENTED_EDGE('',*,*,#2858,.T.);
#3700=ORIENTED_EDGE('',*,*,#2859,.T.);
#3701=ORIENTED_EDGE('',*,*,#2855,.F.);
#3702=ORIENTED_EDGE('',*,*,#2860,.T.);
#3703=ORIENTED_EDGE('',*,*,#2861,.T.);
#3704=ORIENTED_EDGE('',*,*,#2862,.T.);
#3705=ORIENTED_EDGE('',*,*,#2858,.F.);
#3706=ORIENTED_EDGE('',*,*,#2863,.T.);
#3707=ORIENTED_EDGE('',*,*,#2850,.T.);
#3708=ORIENTED_EDGE('',*,*,#2864,.T.);
#3709=ORIENTED_EDGE('',*,*,#2861,.F.);
#3710=ORIENTED_EDGE('',*,*,#2863,.F.);
#3711=ORIENTED_EDGE('',*,*,#2860,.F.);
#3712=ORIENTED_EDGE('',*,*,#2857,.F.);
#3713=ORIENTED_EDGE('',*,*,#2854,.F.);
#3714=ORIENTED_EDGE('',*,*,#2851,.F.);
#3715=ORIENTED_EDGE('',*,*,#2847,.F.);
#3716=ORIENTED_EDGE('',*,*,#2864,.F.);
#3717=ORIENTED_EDGE('',*,*,#2849,.F.);
#3718=ORIENTED_EDGE('',*,*,#2853,.F.);
#3719=ORIENTED_EDGE('',*,*,#2856,.F.);
#3720=ORIENTED_EDGE('',*,*,#2859,.F.);
#3721=ORIENTED_EDGE('',*,*,#2862,.F.);
#3722=ORIENTED_EDGE('',*,*,#2865,.T.);
#3723=ORIENTED_EDGE('',*,*,#2866,.F.);
#3724=ORIENTED_EDGE('',*,*,#2865,.F.);
#3725=ORIENTED_EDGE('',*,*,#2867,.T.);
#3726=ORIENTED_EDGE('',*,*,#2868,.T.);
#3727=ORIENTED_EDGE('',*,*,#2867,.F.);
#3728=ORIENTED_EDGE('',*,*,#2868,.F.);
#3729=ORIENTED_EDGE('',*,*,#2869,.F.);
#3730=ORIENTED_EDGE('',*,*,#2870,.F.);
#3731=ORIENTED_EDGE('',*,*,#2871,.T.);
#3732=ORIENTED_EDGE('',*,*,#2869,.T.);
#3733=ORIENTED_EDGE('',*,*,#2871,.F.);
#3734=ORIENTED_EDGE('',*,*,#2872,.F.);
#3735=ORIENTED_EDGE('',*,*,#2873,.T.);
#3736=ORIENTED_EDGE('',*,*,#2870,.T.);
#3737=ORIENTED_EDGE('',*,*,#2873,.F.);
#3738=ORIENTED_EDGE('',*,*,#2874,.F.);
#3739=ORIENTED_EDGE('',*,*,#2875,.T.);
#3740=ORIENTED_EDGE('',*,*,#2872,.T.);
#3741=ORIENTED_EDGE('',*,*,#2875,.F.);
#3742=ORIENTED_EDGE('',*,*,#2874,.T.);
#3743=ORIENTED_EDGE('',*,*,#2876,.F.);
#3744=ORIENTED_EDGE('',*,*,#2877,.F.);
#3745=ORIENTED_EDGE('',*,*,#2878,.T.);
#3746=ORIENTED_EDGE('',*,*,#2876,.T.);
#3747=ORIENTED_EDGE('',*,*,#2878,.F.);
#3748=ORIENTED_EDGE('',*,*,#2866,.T.);
#3749=ORIENTED_EDGE('',*,*,#2879,.T.);
#3750=ORIENTED_EDGE('',*,*,#2877,.T.);
#3751=ORIENTED_EDGE('',*,*,#2879,.F.);
#3752=ORIENTED_EDGE('',*,*,#2880,.F.);
#3753=ORIENTED_EDGE('',*,*,#2881,.T.);
#3754=ORIENTED_EDGE('',*,*,#2882,.T.);
#3755=ORIENTED_EDGE('',*,*,#2881,.F.);
#3756=ORIENTED_EDGE('',*,*,#2883,.F.);
#3757=ORIENTED_EDGE('',*,*,#2884,.T.);
#3758=ORIENTED_EDGE('',*,*,#2885,.T.);
#3759=ORIENTED_EDGE('',*,*,#2884,.F.);
#3760=ORIENTED_EDGE('',*,*,#2883,.T.);
#3761=ORIENTED_EDGE('',*,*,#2880,.T.);
#3762=ORIENTED_EDGE('',*,*,#2885,.F.);
#3763=ORIENTED_EDGE('',*,*,#2882,.F.);
#3764=ORIENTED_EDGE('',*,*,#2886,.F.);
#3765=ORIENTED_EDGE('',*,*,#2887,.F.);
#3766=ORIENTED_EDGE('',*,*,#2888,.T.);
#3767=ORIENTED_EDGE('',*,*,#2889,.F.);
#3768=ORIENTED_EDGE('',*,*,#2888,.F.);
#3769=ORIENTED_EDGE('',*,*,#2890,.F.);
#3770=ORIENTED_EDGE('',*,*,#2891,.F.);
#3771=ORIENTED_EDGE('',*,*,#2892,.F.);
#3772=ORIENTED_EDGE('',*,*,#2893,.F.);
#3773=ORIENTED_EDGE('',*,*,#2894,.F.);
#3774=ORIENTED_EDGE('',*,*,#2895,.T.);
#3775=ORIENTED_EDGE('',*,*,#2896,.F.);
#3776=ORIENTED_EDGE('',*,*,#2897,.F.);
#3777=ORIENTED_EDGE('',*,*,#2898,.F.);
#3778=ORIENTED_EDGE('',*,*,#2899,.F.);
#3779=ORIENTED_EDGE('',*,*,#2900,.F.);
#3780=ORIENTED_EDGE('',*,*,#2901,.F.);
#3781=ORIENTED_EDGE('',*,*,#2895,.F.);
#3782=ORIENTED_EDGE('',*,*,#2891,.T.);
#3783=ORIENTED_EDGE('',*,*,#2902,.T.);
#3784=ORIENTED_EDGE('',*,*,#2900,.T.);
#3785=ORIENTED_EDGE('',*,*,#2903,.F.);
#3786=ORIENTED_EDGE('',*,*,#2890,.T.);
#3787=ORIENTED_EDGE('',*,*,#2904,.T.);
#3788=ORIENTED_EDGE('',*,*,#2901,.T.);
#3789=ORIENTED_EDGE('',*,*,#2902,.F.);
#3790=ORIENTED_EDGE('',*,*,#2887,.T.);
#3791=ORIENTED_EDGE('',*,*,#2905,.T.);
#3792=ORIENTED_EDGE('',*,*,#2896,.T.);
#3793=ORIENTED_EDGE('',*,*,#2904,.F.);
#3794=ORIENTED_EDGE('',*,*,#2906,.F.);
#3795=ORIENTED_EDGE('',*,*,#2907,.T.);
#3796=ORIENTED_EDGE('',*,*,#2908,.T.);
#3797=ORIENTED_EDGE('',*,*,#2907,.F.);
#3798=ORIENTED_EDGE('',*,*,#2886,.T.);
#3799=ORIENTED_EDGE('',*,*,#2909,.T.);
#3800=ORIENTED_EDGE('',*,*,#2897,.T.);
#3801=ORIENTED_EDGE('',*,*,#2905,.F.);
#3802=ORIENTED_EDGE('',*,*,#2892,.T.);
#3803=ORIENTED_EDGE('',*,*,#2903,.T.);
#3804=ORIENTED_EDGE('',*,*,#2899,.T.);
#3805=ORIENTED_EDGE('',*,*,#2910,.F.);
#3806=ORIENTED_EDGE('',*,*,#2893,.T.);
#3807=ORIENTED_EDGE('',*,*,#2910,.T.);
#3808=ORIENTED_EDGE('',*,*,#2898,.T.);
#3809=ORIENTED_EDGE('',*,*,#2909,.F.);
#3810=ORIENTED_EDGE('',*,*,#2894,.T.);
#3811=ORIENTED_EDGE('',*,*,#2906,.T.);
#3812=ORIENTED_EDGE('',*,*,#2889,.T.);
#3813=ORIENTED_EDGE('',*,*,#2908,.F.);
#3814=ORIENTED_EDGE('',*,*,#2911,.F.);
#3815=ORIENTED_EDGE('',*,*,#2912,.F.);
#3816=ORIENTED_EDGE('',*,*,#2913,.T.);
#3817=ORIENTED_EDGE('',*,*,#2911,.T.);
#3818=ORIENTED_EDGE('',*,*,#2913,.F.);
#3819=ORIENTED_EDGE('',*,*,#2914,.F.);
#3820=ORIENTED_EDGE('',*,*,#2915,.T.);
#3821=ORIENTED_EDGE('',*,*,#2912,.T.);
#3822=ORIENTED_EDGE('',*,*,#2915,.F.);
#3823=ORIENTED_EDGE('',*,*,#2916,.F.);
#3824=ORIENTED_EDGE('',*,*,#2917,.T.);
#3825=ORIENTED_EDGE('',*,*,#2914,.T.);
#3826=ORIENTED_EDGE('',*,*,#2917,.F.);
#3827=ORIENTED_EDGE('',*,*,#2916,.T.);
#3828=ORIENTED_EDGE('',*,*,#2918,.F.);
#3829=ORIENTED_EDGE('',*,*,#2919,.F.);
#3830=ORIENTED_EDGE('',*,*,#2920,.T.);
#3831=ORIENTED_EDGE('',*,*,#2918,.T.);
#3832=ORIENTED_EDGE('',*,*,#2920,.F.);
#3833=ORIENTED_EDGE('',*,*,#2921,.F.);
#3834=ORIENTED_EDGE('',*,*,#2922,.T.);
#3835=ORIENTED_EDGE('',*,*,#2919,.T.);
#3836=ORIENTED_EDGE('',*,*,#2922,.F.);
#3837=ORIENTED_EDGE('',*,*,#2923,.F.);
#3838=ORIENTED_EDGE('',*,*,#2924,.T.);
#3839=ORIENTED_EDGE('',*,*,#2921,.T.);
#3840=ORIENTED_EDGE('',*,*,#2924,.F.);
#3841=ORIENTED_EDGE('',*,*,#2923,.T.);
#3842=ORIENTED_EDGE('',*,*,#2925,.T.);
#3843=ORIENTED_EDGE('',*,*,#2926,.T.);
#3844=ORIENTED_EDGE('',*,*,#2927,.T.);
#3845=ORIENTED_EDGE('',*,*,#2928,.F.);
#3846=ORIENTED_EDGE('',*,*,#2929,.T.);
#3847=ORIENTED_EDGE('',*,*,#2930,.T.);
#3848=ORIENTED_EDGE('',*,*,#2931,.T.);
#3849=ORIENTED_EDGE('',*,*,#2926,.F.);
#3850=ORIENTED_EDGE('',*,*,#2932,.T.);
#3851=ORIENTED_EDGE('',*,*,#2933,.T.);
#3852=ORIENTED_EDGE('',*,*,#2934,.T.);
#3853=ORIENTED_EDGE('',*,*,#2930,.F.);
#3854=ORIENTED_EDGE('',*,*,#2935,.T.);
#3855=ORIENTED_EDGE('',*,*,#2936,.T.);
#3856=ORIENTED_EDGE('',*,*,#2937,.T.);
#3857=ORIENTED_EDGE('',*,*,#2933,.F.);
#3858=ORIENTED_EDGE('',*,*,#2938,.T.);
#3859=ORIENTED_EDGE('',*,*,#2939,.T.);
#3860=ORIENTED_EDGE('',*,*,#2940,.T.);
#3861=ORIENTED_EDGE('',*,*,#2936,.F.);
#3862=ORIENTED_EDGE('',*,*,#2941,.T.);
#3863=ORIENTED_EDGE('',*,*,#2928,.T.);
#3864=ORIENTED_EDGE('',*,*,#2942,.T.);
#3865=ORIENTED_EDGE('',*,*,#2939,.F.);
#3866=ORIENTED_EDGE('',*,*,#2941,.F.);
#3867=ORIENTED_EDGE('',*,*,#2938,.F.);
#3868=ORIENTED_EDGE('',*,*,#2935,.F.);
#3869=ORIENTED_EDGE('',*,*,#2932,.F.);
#3870=ORIENTED_EDGE('',*,*,#2929,.F.);
#3871=ORIENTED_EDGE('',*,*,#2925,.F.);
#3872=ORIENTED_EDGE('',*,*,#2942,.F.);
#3873=ORIENTED_EDGE('',*,*,#2927,.F.);
#3874=ORIENTED_EDGE('',*,*,#2931,.F.);
#3875=ORIENTED_EDGE('',*,*,#2934,.F.);
#3876=ORIENTED_EDGE('',*,*,#2937,.F.);
#3877=ORIENTED_EDGE('',*,*,#2940,.F.);
#3878=ORIENTED_EDGE('',*,*,#2943,.F.);
#3879=ORIENTED_EDGE('',*,*,#2944,.T.);
#3880=ORIENTED_EDGE('',*,*,#2945,.F.);
#3881=ORIENTED_EDGE('',*,*,#2944,.F.);
#3882=ORIENTED_EDGE('',*,*,#2946,.F.);
#3883=ORIENTED_EDGE('',*,*,#2947,.T.);
#3884=ORIENTED_EDGE('',*,*,#2948,.F.);
#3885=ORIENTED_EDGE('',*,*,#2947,.F.);
#3886=ORIENTED_EDGE('',*,*,#2949,.F.);
#3887=ORIENTED_EDGE('',*,*,#2950,.T.);
#3888=ORIENTED_EDGE('',*,*,#2951,.F.);
#3889=ORIENTED_EDGE('',*,*,#2950,.F.);
#3890=ORIENTED_EDGE('',*,*,#2952,.F.);
#3891=ORIENTED_EDGE('',*,*,#2953,.T.);
#3892=ORIENTED_EDGE('',*,*,#2954,.F.);
#3893=ORIENTED_EDGE('',*,*,#2953,.F.);
#3894=ORIENTED_EDGE('',*,*,#2955,.T.);
#3895=ORIENTED_EDGE('',*,*,#2956,.T.);
#3896=ORIENTED_EDGE('',*,*,#2957,.F.);
#3897=ORIENTED_EDGE('',*,*,#2956,.F.);
#3898=ORIENTED_EDGE('',*,*,#2958,.F.);
#3899=ORIENTED_EDGE('',*,*,#2959,.T.);
#3900=ORIENTED_EDGE('',*,*,#2955,.F.);
#3901=ORIENTED_EDGE('',*,*,#2959,.F.);
#3902=ORIENTED_EDGE('',*,*,#2960,.F.);
#3903=ORIENTED_EDGE('',*,*,#2961,.T.);
#3904=ORIENTED_EDGE('',*,*,#2958,.T.);
#3905=ORIENTED_EDGE('',*,*,#2961,.F.);
#3906=ORIENTED_EDGE('',*,*,#2960,.T.);
#3907=ORIENTED_EDGE('',*,*,#2962,.F.);
#3908=ORIENTED_EDGE('',*,*,#2963,.F.);
#3909=ORIENTED_EDGE('',*,*,#2964,.F.);
#3910=ORIENTED_EDGE('',*,*,#2957,.T.);
#3911=ORIENTED_EDGE('',*,*,#2965,.T.);
#3912=ORIENTED_EDGE('',*,*,#2963,.T.);
#3913=ORIENTED_EDGE('',*,*,#2965,.F.);
#3914=ORIENTED_EDGE('',*,*,#2964,.T.);
#3915=ORIENTED_EDGE('',*,*,#2966,.T.);
#3916=ORIENTED_EDGE('',*,*,#2967,.T.);
#3917=ORIENTED_EDGE('',*,*,#2966,.F.);
#3918=ORIENTED_EDGE('',*,*,#2968,.F.);
#3919=ORIENTED_EDGE('',*,*,#2969,.T.);
#3920=ORIENTED_EDGE('',*,*,#2970,.T.);
#3921=ORIENTED_EDGE('',*,*,#2969,.F.);
#3922=ORIENTED_EDGE('',*,*,#2971,.F.);
#3923=ORIENTED_EDGE('',*,*,#2972,.T.);
#3924=ORIENTED_EDGE('',*,*,#2962,.T.);
#3925=ORIENTED_EDGE('',*,*,#2972,.F.);
#3926=ORIENTED_EDGE('',*,*,#2971,.T.);
#3927=ORIENTED_EDGE('',*,*,#2968,.T.);
#3928=ORIENTED_EDGE('',*,*,#2954,.T.);
#3929=ORIENTED_EDGE('',*,*,#2951,.T.);
#3930=ORIENTED_EDGE('',*,*,#2948,.T.);
#3931=ORIENTED_EDGE('',*,*,#2945,.T.);
#3932=ORIENTED_EDGE('',*,*,#2967,.F.);
#3933=ORIENTED_EDGE('',*,*,#2970,.F.);
#3934=ORIENTED_EDGE('',*,*,#2952,.T.);
#3935=ORIENTED_EDGE('',*,*,#2949,.T.);
#3936=ORIENTED_EDGE('',*,*,#2946,.T.);
#3937=ORIENTED_EDGE('',*,*,#2943,.T.);
#3938=ORIENTED_EDGE('',*,*,#2973,.F.);
#3939=ORIENTED_EDGE('',*,*,#2974,.T.);
#3940=ORIENTED_EDGE('',*,*,#2975,.T.);
#3941=ORIENTED_EDGE('',*,*,#2974,.F.);
#3942=ORIENTED_EDGE('',*,*,#2976,.F.);
#3943=ORIENTED_EDGE('',*,*,#2977,.T.);
#3944=ORIENTED_EDGE('',*,*,#2978,.T.);
#3945=ORIENTED_EDGE('',*,*,#2977,.F.);
#3946=ORIENTED_EDGE('',*,*,#2976,.T.);
#3947=ORIENTED_EDGE('',*,*,#2973,.T.);
#3948=ORIENTED_EDGE('',*,*,#2978,.F.);
#3949=ORIENTED_EDGE('',*,*,#2975,.F.);
#3950=ORIENTED_EDGE('',*,*,#2979,.F.);
#3951=ORIENTED_EDGE('',*,*,#2980,.T.);
#3952=ORIENTED_EDGE('',*,*,#2981,.F.);
#3953=ORIENTED_EDGE('',*,*,#2980,.F.);
#3954=ORIENTED_EDGE('',*,*,#2982,.F.);
#3955=ORIENTED_EDGE('',*,*,#2983,.T.);
#3956=ORIENTED_EDGE('',*,*,#2984,.F.);
#3957=ORIENTED_EDGE('',*,*,#2983,.F.);
#3958=ORIENTED_EDGE('',*,*,#2985,.F.);
#3959=ORIENTED_EDGE('',*,*,#2986,.T.);
#3960=ORIENTED_EDGE('',*,*,#2987,.F.);
#3961=ORIENTED_EDGE('',*,*,#2986,.F.);
#3962=ORIENTED_EDGE('',*,*,#2988,.F.);
#3963=ORIENTED_EDGE('',*,*,#2989,.T.);
#3964=ORIENTED_EDGE('',*,*,#2990,.F.);
#3965=ORIENTED_EDGE('',*,*,#2989,.F.);
#3966=ORIENTED_EDGE('',*,*,#2991,.F.);
#3967=ORIENTED_EDGE('',*,*,#2992,.T.);
#3968=ORIENTED_EDGE('',*,*,#2993,.F.);
#3969=ORIENTED_EDGE('',*,*,#2992,.F.);
#3970=ORIENTED_EDGE('',*,*,#2991,.T.);
#3971=ORIENTED_EDGE('',*,*,#2994,.T.);
#3972=ORIENTED_EDGE('',*,*,#2994,.F.);
#3973=ORIENTED_EDGE('',*,*,#2995,.T.);
#3974=ORIENTED_EDGE('',*,*,#2996,.T.);
#3975=ORIENTED_EDGE('',*,*,#2995,.F.);
#3976=ORIENTED_EDGE('',*,*,#2997,.F.);
#3977=ORIENTED_EDGE('',*,*,#2998,.T.);
#3978=ORIENTED_EDGE('',*,*,#2999,.T.);
#3979=ORIENTED_EDGE('',*,*,#2998,.F.);
#3980=ORIENTED_EDGE('',*,*,#2997,.T.);
#3981=ORIENTED_EDGE('',*,*,#2993,.T.);
#3982=ORIENTED_EDGE('',*,*,#2990,.T.);
#3983=ORIENTED_EDGE('',*,*,#2987,.T.);
#3984=ORIENTED_EDGE('',*,*,#2984,.T.);
#3985=ORIENTED_EDGE('',*,*,#2981,.T.);
#3986=ORIENTED_EDGE('',*,*,#2999,.F.);
#3987=ORIENTED_EDGE('',*,*,#2996,.F.);
#3988=ORIENTED_EDGE('',*,*,#2988,.T.);
#3989=ORIENTED_EDGE('',*,*,#2985,.T.);
#3990=ORIENTED_EDGE('',*,*,#2982,.T.);
#3991=ORIENTED_EDGE('',*,*,#2979,.T.);
#3992=ORIENTED_EDGE('',*,*,#3000,.F.);
#3993=ORIENTED_EDGE('',*,*,#3001,.T.);
#3994=ORIENTED_EDGE('',*,*,#3002,.F.);
#3995=ORIENTED_EDGE('',*,*,#3001,.F.);
#3996=ORIENTED_EDGE('',*,*,#3003,.F.);
#3997=ORIENTED_EDGE('',*,*,#3004,.T.);
#3998=ORIENTED_EDGE('',*,*,#3005,.F.);
#3999=ORIENTED_EDGE('',*,*,#3004,.F.);
#4000=ORIENTED_EDGE('',*,*,#3006,.F.);
#4001=ORIENTED_EDGE('',*,*,#3007,.T.);
#4002=ORIENTED_EDGE('',*,*,#3008,.F.);
#4003=ORIENTED_EDGE('',*,*,#3007,.F.);
#4004=ORIENTED_EDGE('',*,*,#3009,.F.);
#4005=ORIENTED_EDGE('',*,*,#3010,.T.);
#4006=ORIENTED_EDGE('',*,*,#3011,.F.);
#4007=ORIENTED_EDGE('',*,*,#3010,.F.);
#4008=ORIENTED_EDGE('',*,*,#3012,.F.);
#4009=ORIENTED_EDGE('',*,*,#3013,.T.);
#4010=ORIENTED_EDGE('',*,*,#3014,.T.);
#4011=ORIENTED_EDGE('',*,*,#3013,.F.);
#4012=ORIENTED_EDGE('',*,*,#3014,.F.);
#4013=ORIENTED_EDGE('',*,*,#3015,.F.);
#4014=ORIENTED_EDGE('',*,*,#3016,.F.);
#4015=ORIENTED_EDGE('',*,*,#3017,.T.);
#4016=ORIENTED_EDGE('',*,*,#3015,.T.);
#4017=ORIENTED_EDGE('',*,*,#3017,.F.);
#4018=ORIENTED_EDGE('',*,*,#3018,.F.);
#4019=ORIENTED_EDGE('',*,*,#3019,.T.);
#4020=ORIENTED_EDGE('',*,*,#3020,.T.);
#4021=ORIENTED_EDGE('',*,*,#3019,.F.);
#4022=ORIENTED_EDGE('',*,*,#3018,.T.);
#4023=ORIENTED_EDGE('',*,*,#3016,.T.);
#4024=ORIENTED_EDGE('',*,*,#3011,.T.);
#4025=ORIENTED_EDGE('',*,*,#3008,.T.);
#4026=ORIENTED_EDGE('',*,*,#3005,.T.);
#4027=ORIENTED_EDGE('',*,*,#3002,.T.);
#4028=ORIENTED_EDGE('',*,*,#3020,.F.);
#4029=ORIENTED_EDGE('',*,*,#3012,.T.);
#4030=ORIENTED_EDGE('',*,*,#3009,.T.);
#4031=ORIENTED_EDGE('',*,*,#3006,.T.);
#4032=ORIENTED_EDGE('',*,*,#3003,.T.);
#4033=ORIENTED_EDGE('',*,*,#3000,.T.);
#4034=ORIENTED_EDGE('',*,*,#3021,.F.);
#4035=ORIENTED_EDGE('',*,*,#3022,.F.);
#4036=ORIENTED_EDGE('',*,*,#3023,.T.);
#4037=ORIENTED_EDGE('',*,*,#3024,.F.);
#4038=ORIENTED_EDGE('',*,*,#3025,.F.);
#4039=ORIENTED_EDGE('',*,*,#3023,.F.);
#4040=ORIENTED_EDGE('',*,*,#3024,.T.);
#4041=ORIENTED_EDGE('',*,*,#3025,.T.);
#4042=ORIENTED_EDGE('',*,*,#3026,.T.);
#4043=ORIENTED_EDGE('',*,*,#3027,.T.);
#4044=ORIENTED_EDGE('',*,*,#3026,.F.);
#4045=ORIENTED_EDGE('',*,*,#3028,.T.);
#4046=ORIENTED_EDGE('',*,*,#3029,.T.);
#4047=ORIENTED_EDGE('',*,*,#3030,.F.);
#4048=ORIENTED_EDGE('',*,*,#3029,.F.);
#4049=ORIENTED_EDGE('',*,*,#3030,.T.);
#4050=ORIENTED_EDGE('',*,*,#3031,.T.);
#4051=ORIENTED_EDGE('',*,*,#3032,.F.);
#4052=ORIENTED_EDGE('',*,*,#3031,.F.);
#4053=ORIENTED_EDGE('',*,*,#3027,.F.);
#4054=ORIENTED_EDGE('',*,*,#3032,.T.);
#4055=ORIENTED_EDGE('',*,*,#3033,.F.);
#4056=ORIENTED_EDGE('',*,*,#3034,.T.);
#4057=ORIENTED_EDGE('',*,*,#3021,.T.);
#4058=ORIENTED_EDGE('',*,*,#3022,.T.);
#4059=ORIENTED_EDGE('',*,*,#3034,.F.);
#4060=ORIENTED_EDGE('',*,*,#3033,.T.);
#4061=ORIENTED_EDGE('',*,*,#3035,.F.);
#4062=ORIENTED_EDGE('',*,*,#3035,.T.);
#4063=ORIENTED_EDGE('',*,*,#3036,.T.);
#4064=ORIENTED_EDGE('',*,*,#3028,.F.);
#4065=ORIENTED_EDGE('',*,*,#3036,.F.);
#4066=ORIENTED_EDGE('',*,*,#3037,.F.);
#4067=ORIENTED_EDGE('',*,*,#3038,.F.);
#4068=ORIENTED_EDGE('',*,*,#3039,.T.);
#4069=ORIENTED_EDGE('',*,*,#3040,.F.);
#4070=ORIENTED_EDGE('',*,*,#3041,.F.);
#4071=ORIENTED_EDGE('',*,*,#3039,.F.);
#4072=ORIENTED_EDGE('',*,*,#3042,.T.);
#4073=ORIENTED_EDGE('',*,*,#3043,.T.);
#4074=ORIENTED_EDGE('',*,*,#3040,.T.);
#4075=ORIENTED_EDGE('',*,*,#3041,.T.);
#4076=ORIENTED_EDGE('',*,*,#3043,.F.);
#4077=ORIENTED_EDGE('',*,*,#3044,.F.);
#4078=ORIENTED_EDGE('',*,*,#3045,.T.);
#4079=ORIENTED_EDGE('',*,*,#3046,.F.);
#4080=ORIENTED_EDGE('',*,*,#3047,.T.);
#4081=ORIENTED_EDGE('',*,*,#3044,.T.);
#4082=ORIENTED_EDGE('',*,*,#3047,.F.);
#4083=ORIENTED_EDGE('',*,*,#3048,.F.);
#4084=ORIENTED_EDGE('',*,*,#3049,.T.);
#4085=ORIENTED_EDGE('',*,*,#3046,.T.);
#4086=ORIENTED_EDGE('',*,*,#3049,.F.);
#4087=ORIENTED_EDGE('',*,*,#3050,.F.);
#4088=ORIENTED_EDGE('',*,*,#3051,.T.);
#4089=ORIENTED_EDGE('',*,*,#3048,.T.);
#4090=ORIENTED_EDGE('',*,*,#3051,.F.);
#4091=ORIENTED_EDGE('',*,*,#3050,.T.);
#4092=ORIENTED_EDGE('',*,*,#3042,.F.);
#4093=ORIENTED_EDGE('',*,*,#3037,.T.);
#4094=ORIENTED_EDGE('',*,*,#3038,.T.);
#4095=ORIENTED_EDGE('',*,*,#3052,.T.);
#4096=ORIENTED_EDGE('',*,*,#3045,.F.);
#4097=ORIENTED_EDGE('',*,*,#3052,.F.);
#4098=ORIENTED_EDGE('',*,*,#3053,.T.);
#4099=ORIENTED_EDGE('',*,*,#3053,.F.);
#4100=ORIENTED_EDGE('',*,*,#3054,.T.);
#4101=ORIENTED_EDGE('',*,*,#3054,.F.);
#4102=ORIENTED_EDGE('',*,*,#3055,.T.);
#4103=ORIENTED_EDGE('',*,*,#3055,.F.);
#4104=ORIENTED_EDGE('',*,*,#3056,.T.);
#4105=ORIENTED_EDGE('',*,*,#3056,.F.);
#4106=ORIENTED_EDGE('',*,*,#3057,.T.);
#4107=ORIENTED_EDGE('',*,*,#3057,.F.);
#4108=ORIENTED_EDGE('',*,*,#3058,.T.);
#4109=ORIENTED_EDGE('',*,*,#3058,.F.);
#4110=ORIENTED_EDGE('',*,*,#3059,.T.);
#4111=ORIENTED_EDGE('',*,*,#3059,.F.);
#4112=ORIENTED_EDGE('',*,*,#3060,.T.);
#4113=ORIENTED_EDGE('',*,*,#3060,.F.);
#4114=ORIENTED_EDGE('',*,*,#3061,.F.);
#4115=ORIENTED_EDGE('',*,*,#3062,.F.);
#4116=ORIENTED_EDGE('',*,*,#3063,.F.);
#4117=ORIENTED_EDGE('',*,*,#3064,.F.);
#4118=ORIENTED_EDGE('',*,*,#3063,.T.);
#4119=ORIENTED_EDGE('',*,*,#3065,.F.);
#4120=ORIENTED_EDGE('',*,*,#3066,.T.);
#4121=ORIENTED_EDGE('',*,*,#3067,.F.);
#4122=ORIENTED_EDGE('',*,*,#3068,.T.);
#4123=ORIENTED_EDGE('',*,*,#3069,.F.);
#4124=ORIENTED_EDGE('',*,*,#3070,.T.);
#4125=ORIENTED_EDGE('',*,*,#3071,.T.);
#4126=ORIENTED_EDGE('',*,*,#3072,.F.);
#4127=ORIENTED_EDGE('',*,*,#3071,.F.);
#4128=ORIENTED_EDGE('',*,*,#3073,.T.);
#4129=ORIENTED_EDGE('',*,*,#3074,.F.);
#4130=ORIENTED_EDGE('',*,*,#3075,.T.);
#4131=ORIENTED_EDGE('',*,*,#3076,.F.);
#4132=ORIENTED_EDGE('',*,*,#3077,.T.);
#4133=ORIENTED_EDGE('',*,*,#3078,.F.);
#4134=ORIENTED_EDGE('',*,*,#3079,.T.);
#4135=ORIENTED_EDGE('',*,*,#3080,.F.);
#4136=ORIENTED_EDGE('',*,*,#3081,.T.);
#4137=ORIENTED_EDGE('',*,*,#3082,.F.);
#4138=ORIENTED_EDGE('',*,*,#3062,.T.);
#4139=ORIENTED_EDGE('',*,*,#3083,.T.);
#4140=ORIENTED_EDGE('',*,*,#3084,.T.);
#4141=ORIENTED_EDGE('',*,*,#3065,.T.);
#4142=ORIENTED_EDGE('',*,*,#3085,.F.);
#4143=ORIENTED_EDGE('',*,*,#3086,.F.);
#4144=ORIENTED_EDGE('',*,*,#3066,.F.);
#4145=ORIENTED_EDGE('',*,*,#3084,.F.);
#4146=ORIENTED_EDGE('',*,*,#3086,.T.);
#4147=ORIENTED_EDGE('',*,*,#3087,.T.);
#4148=ORIENTED_EDGE('',*,*,#3088,.T.);
#4149=ORIENTED_EDGE('',*,*,#3067,.T.);
#4150=ORIENTED_EDGE('',*,*,#3089,.F.);
#4151=ORIENTED_EDGE('',*,*,#3090,.F.);
#4152=ORIENTED_EDGE('',*,*,#3068,.F.);
#4153=ORIENTED_EDGE('',*,*,#3088,.F.);
#4154=ORIENTED_EDGE('',*,*,#3090,.T.);
#4155=ORIENTED_EDGE('',*,*,#3091,.T.);
#4156=ORIENTED_EDGE('',*,*,#3092,.T.);
#4157=ORIENTED_EDGE('',*,*,#3069,.T.);
#4158=ORIENTED_EDGE('',*,*,#3093,.F.);
#4159=ORIENTED_EDGE('',*,*,#3094,.F.);
#4160=ORIENTED_EDGE('',*,*,#3073,.F.);
#4161=ORIENTED_EDGE('',*,*,#3070,.F.);
#4162=ORIENTED_EDGE('',*,*,#3092,.F.);
#4163=ORIENTED_EDGE('',*,*,#3095,.F.);
#4164=ORIENTED_EDGE('',*,*,#3094,.T.);
#4165=ORIENTED_EDGE('',*,*,#3096,.T.);
#4166=ORIENTED_EDGE('',*,*,#3097,.T.);
#4167=ORIENTED_EDGE('',*,*,#3074,.T.);
#4168=ORIENTED_EDGE('',*,*,#3098,.F.);
#4169=ORIENTED_EDGE('',*,*,#3099,.F.);
#4170=ORIENTED_EDGE('',*,*,#3075,.F.);
#4171=ORIENTED_EDGE('',*,*,#3097,.F.);
#4172=ORIENTED_EDGE('',*,*,#3099,.T.);
#4173=ORIENTED_EDGE('',*,*,#3100,.T.);
#4174=ORIENTED_EDGE('',*,*,#3101,.T.);
#4175=ORIENTED_EDGE('',*,*,#3076,.T.);
#4176=ORIENTED_EDGE('',*,*,#3102,.F.);
#4177=ORIENTED_EDGE('',*,*,#3103,.F.);
#4178=ORIENTED_EDGE('',*,*,#3077,.F.);
#4179=ORIENTED_EDGE('',*,*,#3101,.F.);
#4180=ORIENTED_EDGE('',*,*,#3103,.T.);
#4181=ORIENTED_EDGE('',*,*,#3104,.T.);
#4182=ORIENTED_EDGE('',*,*,#3105,.T.);
#4183=ORIENTED_EDGE('',*,*,#3078,.T.);
#4184=ORIENTED_EDGE('',*,*,#3079,.F.);
#4185=ORIENTED_EDGE('',*,*,#3105,.F.);
#4186=ORIENTED_EDGE('',*,*,#3106,.F.);
#4187=ORIENTED_EDGE('',*,*,#3107,.F.);
#4188=ORIENTED_EDGE('',*,*,#3108,.F.);
#4189=ORIENTED_EDGE('',*,*,#3109,.T.);
#4190=ORIENTED_EDGE('',*,*,#3095,.T.);
#4191=ORIENTED_EDGE('',*,*,#3091,.F.);
#4192=ORIENTED_EDGE('',*,*,#3089,.T.);
#4193=ORIENTED_EDGE('',*,*,#3087,.F.);
#4194=ORIENTED_EDGE('',*,*,#3085,.T.);
#4195=ORIENTED_EDGE('',*,*,#3083,.F.);
#4196=ORIENTED_EDGE('',*,*,#3061,.T.);
#4197=ORIENTED_EDGE('',*,*,#3110,.F.);
#4198=ORIENTED_EDGE('',*,*,#3111,.T.);
#4199=ORIENTED_EDGE('',*,*,#3112,.F.);
#4200=ORIENTED_EDGE('',*,*,#3106,.T.);
#4201=ORIENTED_EDGE('',*,*,#3104,.F.);
#4202=ORIENTED_EDGE('',*,*,#3102,.T.);
#4203=ORIENTED_EDGE('',*,*,#3100,.F.);
#4204=ORIENTED_EDGE('',*,*,#3098,.T.);
#4205=ORIENTED_EDGE('',*,*,#3096,.F.);
#4206=ORIENTED_EDGE('',*,*,#3093,.T.);
#4207=ORIENTED_EDGE('',*,*,#3109,.F.);
#4208=ORIENTED_EDGE('',*,*,#3064,.T.);
#4209=ORIENTED_EDGE('',*,*,#3082,.T.);
#4210=ORIENTED_EDGE('',*,*,#3113,.T.);
#4211=ORIENTED_EDGE('',*,*,#3110,.T.);
#4212=ORIENTED_EDGE('',*,*,#3081,.F.);
#4213=ORIENTED_EDGE('',*,*,#3114,.F.);
#4214=ORIENTED_EDGE('',*,*,#3111,.F.);
#4215=ORIENTED_EDGE('',*,*,#3113,.F.);
#4216=ORIENTED_EDGE('',*,*,#3072,.T.);
#4217=ORIENTED_EDGE('',*,*,#3108,.T.);
#4218=ORIENTED_EDGE('',*,*,#3107,.T.);
#4219=ORIENTED_EDGE('',*,*,#3112,.T.);
#4220=ORIENTED_EDGE('',*,*,#3114,.T.);
#4221=ORIENTED_EDGE('',*,*,#3080,.T.);
#4222=ORIENTED_EDGE('',*,*,#3115,.F.);
#4223=ORIENTED_EDGE('',*,*,#3116,.T.);
#4224=ORIENTED_EDGE('',*,*,#3117,.F.);
#4225=ORIENTED_EDGE('',*,*,#3118,.T.);
#4226=ORIENTED_EDGE('',*,*,#3115,.T.);
#4227=ORIENTED_EDGE('',*,*,#3118,.F.);
#4228=ORIENTED_EDGE('',*,*,#3117,.T.);
#4229=ORIENTED_EDGE('',*,*,#3119,.F.);
#4230=ORIENTED_EDGE('',*,*,#3119,.T.);
#4231=ORIENTED_EDGE('',*,*,#3120,.T.);
#4232=ORIENTED_EDGE('',*,*,#3116,.F.);
#4233=ORIENTED_EDGE('',*,*,#3120,.F.);
#4234=ORIENTED_EDGE('',*,*,#3121,.F.);
#4235=ORIENTED_EDGE('',*,*,#3122,.T.);
#4236=ORIENTED_EDGE('',*,*,#3123,.F.);
#4237=ORIENTED_EDGE('',*,*,#3124,.T.);
#4238=ORIENTED_EDGE('',*,*,#3121,.T.);
#4239=ORIENTED_EDGE('',*,*,#3124,.F.);
#4240=ORIENTED_EDGE('',*,*,#3123,.T.);
#4241=ORIENTED_EDGE('',*,*,#3125,.F.);
#4242=ORIENTED_EDGE('',*,*,#3125,.T.);
#4243=ORIENTED_EDGE('',*,*,#3126,.T.);
#4244=ORIENTED_EDGE('',*,*,#3122,.F.);
#4245=ORIENTED_EDGE('',*,*,#3126,.F.);
#4246=ORIENTED_EDGE('',*,*,#3127,.T.);
#4247=ORIENTED_EDGE('',*,*,#3128,.T.);
#4248=ORIENTED_EDGE('',*,*,#3129,.T.);
#4249=ORIENTED_EDGE('',*,*,#3130,.F.);
#4250=ORIENTED_EDGE('',*,*,#3131,.T.);
#4251=ORIENTED_EDGE('',*,*,#3132,.T.);
#4252=ORIENTED_EDGE('',*,*,#3133,.T.);
#4253=ORIENTED_EDGE('',*,*,#3128,.F.);
#4254=ORIENTED_EDGE('',*,*,#3134,.T.);
#4255=ORIENTED_EDGE('',*,*,#3135,.T.);
#4256=ORIENTED_EDGE('',*,*,#3136,.T.);
#4257=ORIENTED_EDGE('',*,*,#3132,.F.);
#4258=ORIENTED_EDGE('',*,*,#3137,.T.);
#4259=ORIENTED_EDGE('',*,*,#3138,.T.);
#4260=ORIENTED_EDGE('',*,*,#3139,.T.);
#4261=ORIENTED_EDGE('',*,*,#3135,.F.);
#4262=ORIENTED_EDGE('',*,*,#3140,.T.);
#4263=ORIENTED_EDGE('',*,*,#3141,.T.);
#4264=ORIENTED_EDGE('',*,*,#3142,.T.);
#4265=ORIENTED_EDGE('',*,*,#3138,.F.);
#4266=ORIENTED_EDGE('',*,*,#3143,.T.);
#4267=ORIENTED_EDGE('',*,*,#3130,.T.);
#4268=ORIENTED_EDGE('',*,*,#3144,.T.);
#4269=ORIENTED_EDGE('',*,*,#3141,.F.);
#4270=ORIENTED_EDGE('',*,*,#3143,.F.);
#4271=ORIENTED_EDGE('',*,*,#3140,.F.);
#4272=ORIENTED_EDGE('',*,*,#3137,.F.);
#4273=ORIENTED_EDGE('',*,*,#3134,.F.);
#4274=ORIENTED_EDGE('',*,*,#3131,.F.);
#4275=ORIENTED_EDGE('',*,*,#3127,.F.);
#4276=ORIENTED_EDGE('',*,*,#3144,.F.);
#4277=ORIENTED_EDGE('',*,*,#3129,.F.);
#4278=ORIENTED_EDGE('',*,*,#3133,.F.);
#4279=ORIENTED_EDGE('',*,*,#3136,.F.);
#4280=ORIENTED_EDGE('',*,*,#3139,.F.);
#4281=ORIENTED_EDGE('',*,*,#3142,.F.);
#4282=ORIENTED_EDGE('',*,*,#3145,.F.);
#4283=ORIENTED_EDGE('',*,*,#3146,.F.);
#4284=ORIENTED_EDGE('',*,*,#3147,.F.);
#4285=ORIENTED_EDGE('',*,*,#3148,.T.);
#4286=ORIENTED_EDGE('',*,*,#3146,.T.);
#4287=ORIENTED_EDGE('',*,*,#3148,.F.);
#4288=ORIENTED_EDGE('',*,*,#3149,.F.);
#4289=ORIENTED_EDGE('',*,*,#3150,.T.);
#4290=ORIENTED_EDGE('',*,*,#3147,.T.);
#4291=ORIENTED_EDGE('',*,*,#3150,.F.);
#4292=ORIENTED_EDGE('',*,*,#3151,.F.);
#4293=ORIENTED_EDGE('',*,*,#3152,.T.);
#4294=ORIENTED_EDGE('',*,*,#3149,.T.);
#4295=ORIENTED_EDGE('',*,*,#3152,.F.);
#4296=ORIENTED_EDGE('',*,*,#3151,.T.);
#4297=ORIENTED_EDGE('',*,*,#3153,.F.);
#4298=ORIENTED_EDGE('',*,*,#3154,.F.);
#4299=ORIENTED_EDGE('',*,*,#3155,.T.);
#4300=ORIENTED_EDGE('',*,*,#3153,.T.);
#4301=ORIENTED_EDGE('',*,*,#3155,.F.);
#4302=ORIENTED_EDGE('',*,*,#3145,.T.);
#4303=ORIENTED_EDGE('',*,*,#3156,.T.);
#4304=ORIENTED_EDGE('',*,*,#3154,.T.);
#4305=ORIENTED_EDGE('',*,*,#3156,.F.);
#4306=ORIENTED_EDGE('',*,*,#3157,.T.);
#4307=ORIENTED_EDGE('',*,*,#3158,.F.);
#4308=ORIENTED_EDGE('',*,*,#3159,.F.);
#4309=ORIENTED_EDGE('',*,*,#3160,.F.);
#4310=ORIENTED_EDGE('',*,*,#3157,.F.);
#4311=ORIENTED_EDGE('',*,*,#3161,.T.);
#4312=ORIENTED_EDGE('',*,*,#3159,.T.);
#4313=ORIENTED_EDGE('',*,*,#3161,.F.);
#4314=ORIENTED_EDGE('',*,*,#3160,.T.);
#4315=ORIENTED_EDGE('',*,*,#3162,.T.);
#4316=ORIENTED_EDGE('',*,*,#3163,.F.);
#4317=ORIENTED_EDGE('',*,*,#3164,.F.);
#4318=ORIENTED_EDGE('',*,*,#3165,.F.);
#4319=ORIENTED_EDGE('',*,*,#3162,.F.);
#4320=ORIENTED_EDGE('',*,*,#3166,.F.);
#4321=ORIENTED_EDGE('',*,*,#3167,.T.);
#4322=ORIENTED_EDGE('',*,*,#3158,.T.);
#4323=ORIENTED_EDGE('',*,*,#3167,.F.);
#4324=ORIENTED_EDGE('',*,*,#3166,.T.);
#4325=ORIENTED_EDGE('',*,*,#3164,.T.);
#4326=ORIENTED_EDGE('',*,*,#3168,.F.);
#4327=ORIENTED_EDGE('',*,*,#3169,.T.);
#4328=ORIENTED_EDGE('',*,*,#3170,.F.);
#4329=ORIENTED_EDGE('',*,*,#3163,.T.);
#4330=ORIENTED_EDGE('',*,*,#3165,.T.);
#4331=ORIENTED_EDGE('',*,*,#3171,.F.);
#4332=ORIENTED_EDGE('',*,*,#3172,.F.);
#4333=ORIENTED_EDGE('',*,*,#3173,.F.);
#4334=ORIENTED_EDGE('',*,*,#3174,.F.);
#4335=ORIENTED_EDGE('',*,*,#3175,.F.);
#4336=ORIENTED_EDGE('',*,*,#3172,.T.);
#4337=ORIENTED_EDGE('',*,*,#3176,.F.);
#4338=ORIENTED_EDGE('',*,*,#3177,.F.);
#4339=ORIENTED_EDGE('',*,*,#3178,.F.);
#4340=ORIENTED_EDGE('',*,*,#3179,.F.);
#4341=ORIENTED_EDGE('',*,*,#3180,.F.);
#4342=ORIENTED_EDGE('',*,*,#3181,.T.);
#4343=ORIENTED_EDGE('',*,*,#3178,.T.);
#4344=ORIENTED_EDGE('',*,*,#3182,.T.);
#4345=ORIENTED_EDGE('',*,*,#3183,.T.);
#4346=ORIENTED_EDGE('',*,*,#3184,.T.);
#4347=ORIENTED_EDGE('',*,*,#3176,.T.);
#4348=ORIENTED_EDGE('',*,*,#3171,.T.);
#4349=ORIENTED_EDGE('',*,*,#3170,.T.);
#4350=ORIENTED_EDGE('',*,*,#3177,.T.);
#4351=ORIENTED_EDGE('',*,*,#3185,.T.);
#4352=ORIENTED_EDGE('',*,*,#3186,.T.);
#4353=ORIENTED_EDGE('',*,*,#3182,.F.);
#4354=ORIENTED_EDGE('',*,*,#3187,.T.);
#4355=ORIENTED_EDGE('',*,*,#3168,.T.);
#4356=ORIENTED_EDGE('',*,*,#3173,.T.);
#4357=ORIENTED_EDGE('',*,*,#3175,.T.);
#4358=ORIENTED_EDGE('',*,*,#3188,.F.);
#4359=ORIENTED_EDGE('',*,*,#3189,.T.);
#4360=ORIENTED_EDGE('',*,*,#3185,.F.);
#4361=ORIENTED_EDGE('',*,*,#3180,.T.);
#4362=ORIENTED_EDGE('',*,*,#3187,.F.);
#4363=ORIENTED_EDGE('',*,*,#3179,.T.);
#4364=ORIENTED_EDGE('',*,*,#3181,.F.);
#4365=ORIENTED_EDGE('',*,*,#3169,.F.);
#4366=ORIENTED_EDGE('',*,*,#3190,.F.);
#4367=ORIENTED_EDGE('',*,*,#3183,.F.);
#4368=ORIENTED_EDGE('',*,*,#3186,.F.);
#4369=ORIENTED_EDGE('',*,*,#3189,.F.);
#4370=ORIENTED_EDGE('',*,*,#3174,.T.);
#4371=ORIENTED_EDGE('',*,*,#3184,.F.);
#4372=ORIENTED_EDGE('',*,*,#3190,.T.);
#4373=ORIENTED_EDGE('',*,*,#3188,.T.);
#4374=ORIENTED_EDGE('',*,*,#3191,.F.);
#4375=ORIENTED_EDGE('',*,*,#3192,.T.);
#4376=ORIENTED_EDGE('',*,*,#3193,.T.);
#4377=ORIENTED_EDGE('',*,*,#3192,.F.);
#4378=ORIENTED_EDGE('',*,*,#3194,.F.);
#4379=ORIENTED_EDGE('',*,*,#3195,.T.);
#4380=ORIENTED_EDGE('',*,*,#3196,.T.);
#4381=ORIENTED_EDGE('',*,*,#3195,.F.);
#4382=ORIENTED_EDGE('',*,*,#3194,.T.);
#4383=ORIENTED_EDGE('',*,*,#3191,.T.);
#4384=ORIENTED_EDGE('',*,*,#3196,.F.);
#4385=ORIENTED_EDGE('',*,*,#3193,.F.);
#4386=ORIENTED_EDGE('',*,*,#3197,.F.);
#4387=ORIENTED_EDGE('',*,*,#3198,.T.);
#4388=ORIENTED_EDGE('',*,*,#3199,.F.);
#4389=ORIENTED_EDGE('',*,*,#3198,.F.);
#4390=ORIENTED_EDGE('',*,*,#3200,.T.);
#4391=ORIENTED_EDGE('',*,*,#3201,.T.);
#4392=ORIENTED_EDGE('',*,*,#3202,.F.);
#4393=ORIENTED_EDGE('',*,*,#3203,.F.);
#4394=ORIENTED_EDGE('',*,*,#3204,.T.);
#4395=ORIENTED_EDGE('',*,*,#3203,.T.);
#4396=ORIENTED_EDGE('',*,*,#3205,.F.);
#4397=ORIENTED_EDGE('',*,*,#3206,.F.);
#4398=ORIENTED_EDGE('',*,*,#3207,.T.);
#4399=ORIENTED_EDGE('',*,*,#3206,.T.);
#4400=ORIENTED_EDGE('',*,*,#3208,.F.);
#4401=ORIENTED_EDGE('',*,*,#3209,.F.);
#4402=ORIENTED_EDGE('',*,*,#3210,.T.);
#4403=ORIENTED_EDGE('',*,*,#3209,.T.);
#4404=ORIENTED_EDGE('',*,*,#3211,.F.);
#4405=ORIENTED_EDGE('',*,*,#3212,.F.);
#4406=ORIENTED_EDGE('',*,*,#3213,.T.);
#4407=ORIENTED_EDGE('',*,*,#3212,.T.);
#4408=ORIENTED_EDGE('',*,*,#3214,.F.);
#4409=ORIENTED_EDGE('',*,*,#3215,.F.);
#4410=ORIENTED_EDGE('',*,*,#3216,.T.);
#4411=ORIENTED_EDGE('',*,*,#3215,.T.);
#4412=ORIENTED_EDGE('',*,*,#3217,.F.);
#4413=ORIENTED_EDGE('',*,*,#3201,.F.);
#4414=ORIENTED_EDGE('',*,*,#3217,.T.);
#4415=ORIENTED_EDGE('',*,*,#3214,.T.);
#4416=ORIENTED_EDGE('',*,*,#3211,.T.);
#4417=ORIENTED_EDGE('',*,*,#3208,.T.);
#4418=ORIENTED_EDGE('',*,*,#3205,.T.);
#4419=ORIENTED_EDGE('',*,*,#3202,.T.);
#4420=ORIENTED_EDGE('',*,*,#3199,.T.);
#4421=ORIENTED_EDGE('',*,*,#3216,.F.);
#4422=ORIENTED_EDGE('',*,*,#3200,.F.);
#4423=ORIENTED_EDGE('',*,*,#3204,.F.);
#4424=ORIENTED_EDGE('',*,*,#3207,.F.);
#4425=ORIENTED_EDGE('',*,*,#3210,.F.);
#4426=ORIENTED_EDGE('',*,*,#3213,.F.);
#4427=ORIENTED_EDGE('',*,*,#3197,.T.);
#4428=ORIENTED_EDGE('',*,*,#3218,.F.);
#4429=ORIENTED_EDGE('',*,*,#3219,.T.);
#4430=ORIENTED_EDGE('',*,*,#3220,.F.);
#4431=ORIENTED_EDGE('',*,*,#3219,.F.);
#4432=ORIENTED_EDGE('',*,*,#3221,.F.);
#4433=ORIENTED_EDGE('',*,*,#3222,.T.);
#4434=ORIENTED_EDGE('',*,*,#3223,.F.);
#4435=ORIENTED_EDGE('',*,*,#3222,.F.);
#4436=ORIENTED_EDGE('',*,*,#3224,.F.);
#4437=ORIENTED_EDGE('',*,*,#3225,.T.);
#4438=ORIENTED_EDGE('',*,*,#3226,.F.);
#4439=ORIENTED_EDGE('',*,*,#3227,.F.);
#4440=ORIENTED_EDGE('',*,*,#3228,.T.);
#4441=ORIENTED_EDGE('',*,*,#3227,.T.);
#4442=ORIENTED_EDGE('',*,*,#3220,.T.);
#4443=ORIENTED_EDGE('',*,*,#3223,.T.);
#4444=ORIENTED_EDGE('',*,*,#3224,.T.);
#4445=ORIENTED_EDGE('',*,*,#3228,.F.);
#4446=ORIENTED_EDGE('',*,*,#3226,.T.);
#4447=ORIENTED_EDGE('',*,*,#3229,.T.);
#4448=ORIENTED_EDGE('',*,*,#3229,.F.);
#4449=ORIENTED_EDGE('',*,*,#3225,.F.);
#4450=ORIENTED_EDGE('',*,*,#3218,.T.);
#4451=ORIENTED_EDGE('',*,*,#3221,.T.);
#4452=PLANE('',#5262);
#4453=PLANE('',#5294);
#4454=PLANE('',#5311);
#4455=PLANE('',#5312);
#4456=PLANE('',#5313);
#4457=PLANE('',#5314);
#4458=PLANE('',#5315);
#4459=PLANE('',#5316);
#4460=PLANE('',#5317);
#4461=PLANE('',#5318);
#4462=PLANE('',#5319);
#4463=PLANE('',#5320);
#4464=PLANE('',#5322);
#4465=PLANE('',#5350);
#4466=PLANE('',#5371);
#4467=PLANE('',#5372);
#4468=PLANE('',#5373);
#4469=PLANE('',#5374);
#4470=PLANE('',#5375);
#4471=PLANE('',#5376);
#4472=PLANE('',#5377);
#4473=PLANE('',#5378);
#4474=PLANE('',#5379);
#4475=PLANE('',#5380);
#4476=PLANE('',#5391);
#4477=PLANE('',#5392);
#4478=PLANE('',#5393);
#4479=PLANE('',#5394);
#4480=PLANE('',#5395);
#4481=PLANE('',#5396);
#4482=PLANE('',#5404);
#4483=PLANE('',#5405);
#4484=PLANE('',#5410);
#4485=PLANE('',#5411);
#4486=PLANE('',#5416);
#4487=PLANE('',#5419);
#4488=PLANE('',#5427);
#4489=PLANE('',#5428);
#4490=PLANE('',#5436);
#4491=PLANE('',#5437);
#4492=PLANE('',#5445);
#4493=PLANE('',#5446);
#4494=PLANE('',#5454);
#4495=PLANE('',#5455);
#4496=PLANE('',#5463);
#4497=PLANE('',#5464);
#4498=PLANE('',#5472);
#4499=PLANE('',#5473);
#4500=PLANE('',#5481);
#4501=PLANE('',#5482);
#4502=PLANE('',#5484);
#4503=PLANE('',#5485);
#4504=PLANE('',#5486);
#4505=PLANE('',#5487);
#4506=PLANE('',#5488);
#4507=PLANE('',#5489);
#4508=PLANE('',#5490);
#4509=PLANE('',#5491);
#4510=PLANE('',#5492);
#4511=PLANE('',#5497);
#4512=PLANE('',#5498);
#4513=PLANE('',#5506);
#4514=PLANE('',#5518);
#4515=PLANE('',#5519);
#4516=PLANE('',#5525);
#4517=PLANE('',#5526);
#4518=PLANE('',#5527);
#4519=PLANE('',#5531);
#4520=PLANE('',#5532);
#4521=PLANE('',#5533);
#4522=PLANE('',#5534);
#4523=PLANE('',#5535);
#4524=PLANE('',#5537);
#4525=PLANE('',#5545);
#4526=PLANE('',#5553);
#4527=PLANE('',#5554);
#4528=PLANE('',#5555);
#4529=PLANE('',#5556);
#4530=PLANE('',#5557);
#4531=PLANE('',#5558);
#4532=PLANE('',#5559);
#4533=PLANE('',#5560);
#4534=PLANE('',#5561);
#4535=PLANE('',#5608);
#4536=PLANE('',#5610);
#4537=PLANE('',#5621);
#4538=PLANE('',#5622);
#4539=PLANE('',#5630);
#4540=PLANE('',#5631);
#4541=PLANE('',#5648);
#4542=PLANE('',#5655);
#4543=PLANE('',#5656);
#4544=PLANE('',#5673);
#4545=PLANE('',#5680);
#4546=PLANE('',#5681);
#4547=PLANE('',#5697);
#4548=PLANE('',#5700);
#4549=PLANE('',#5712);
#4550=PLANE('',#5721);
#4551=PLANE('',#5754);
#4552=PLANE('',#5759);
#4553=PLANE('',#5764);
#4554=PLANE('',#5769);
#4555=PLANE('',#5774);
#4556=PLANE('',#5779);
#4557=PLANE('',#5788);
#4558=PLANE('',#5792);
#4559=PLANE('',#5793);
#4560=PLANE('',#5795);
#4561=PLANE('',#5800);
#4562=PLANE('',#5803);
#4563=PLANE('',#5808);
#4564=PLANE('',#5817);
#4565=PLANE('',#5818);
#4566=PLANE('',#5819);
#4567=PLANE('',#5820);
#4568=PLANE('',#5821);
#4569=PLANE('',#5822);
#4570=PLANE('',#5823);
#4571=PLANE('',#5824);
#4572=PLANE('',#5825);
#4573=PLANE('',#5827);
#4574=PLANE('',#5835);
#4575=PLANE('',#5856);
#4576=PLANE('',#5859);
#4577=PLANE('',#5869);
#4578=PLANE('',#5870);
#4579=PLANE('',#5871);
#4580=PLANE('',#5872);
#4581=PLANE('',#5873);
#4582=PLANE('',#5874);
#4583=PLANE('',#5879);
#4584=PLANE('',#5881);
#4585=PLANE('',#5882);
#4586=PLANE('',#5891);
#4587=PLANE('',#5892);
#4588=PLANE('',#5897);
#4589=PLANE('',#5898);
#4590=PLANE('',#5899);
#4591=PLANE('',#5900);
#4592=PLANE('',#5901);
#4593=PLANE('',#5902);
#4594=PLANE('',#5903);
#4595=PLANE('',#5904);
#4596=PLANE('',#5919);
#4597=PLANE('',#5923);
#4598=ADVANCED_FACE('',(#1222,#1107),#4452,.T.);
#4599=ADVANCED_FACE('',(#1223),#1000,.F.);
#4600=ADVANCED_FACE('',(#1224),#1001,.F.);
#4601=ADVANCED_FACE('',(#1225),#1002,.F.);
#4602=ADVANCED_FACE('',(#1226),#1003,.T.);
#4603=ADVANCED_FACE('',(#1227),#1004,.F.);
#4604=ADVANCED_FACE('',(#1228),#1005,.F.);
#4605=ADVANCED_FACE('',(#1229),#1006,.F.);
#4606=ADVANCED_FACE('',(#1230),#1007,.F.);
#4607=ADVANCED_FACE('',(#1231,#1108),#4453,.T.);
#4608=ADVANCED_FACE('',(#1232),#1008,.F.);
#4609=ADVANCED_FACE('',(#1233),#1009,.F.);
#4610=ADVANCED_FACE('',(#1234),#1010,.F.);
#4611=ADVANCED_FACE('',(#1235),#1011,.F.);
#4612=ADVANCED_FACE('',(#1236),#1012,.F.);
#4613=ADVANCED_FACE('',(#1237),#4454,.T.);
#4614=ADVANCED_FACE('',(#1238),#4455,.T.);
#4615=ADVANCED_FACE('',(#1239),#4456,.T.);
#4616=ADVANCED_FACE('',(#1240),#4457,.T.);
#4617=ADVANCED_FACE('',(#1241),#4458,.T.);
#4618=ADVANCED_FACE('',(#1242),#4459,.T.);
#4619=ADVANCED_FACE('',(#1243),#4460,.T.);
#4620=ADVANCED_FACE('',(#1244),#4461,.T.);
#4621=ADVANCED_FACE('',(#1245,#1109,#1110,#1111,#1112),#4462,.T.);
#4622=ADVANCED_FACE('',(#1246,#1113,#1114,#1115,#1116,#1117,#1118,#1119,
#1120),#4463,.F.);
#4623=ADVANCED_FACE('',(#1247,#1121),#4464,.F.);
#4624=ADVANCED_FACE('',(#1248),#1013,.F.);
#4625=ADVANCED_FACE('',(#1249),#1014,.F.);
#4626=ADVANCED_FACE('',(#1250),#1015,.F.);
#4627=ADVANCED_FACE('',(#1251),#1016,.T.);
#4628=ADVANCED_FACE('',(#1252),#1017,.F.);
#4629=ADVANCED_FACE('',(#1253),#1018,.F.);
#4630=ADVANCED_FACE('',(#1254),#1019,.F.);
#4631=ADVANCED_FACE('',(#1255,#1122),#4465,.F.);
#4632=ADVANCED_FACE('',(#1256),#1020,.F.);
#4633=ADVANCED_FACE('',(#1257),#1021,.F.);
#4634=ADVANCED_FACE('',(#1258),#1022,.F.);
#4635=ADVANCED_FACE('',(#1259),#1023,.F.);
#4636=ADVANCED_FACE('',(#1260),#1024,.F.);
#4637=ADVANCED_FACE('',(#1261),#1025,.F.);
#4638=ADVANCED_FACE('',(#1262),#4466,.T.);
#4639=ADVANCED_FACE('',(#1263),#4467,.T.);
#4640=ADVANCED_FACE('',(#1264),#4468,.T.);
#4641=ADVANCED_FACE('',(#1265),#4469,.T.);
#4642=ADVANCED_FACE('',(#1266),#4470,.T.);
#4643=ADVANCED_FACE('',(#1267),#4471,.T.);
#4644=ADVANCED_FACE('',(#1268),#4472,.T.);
#4645=ADVANCED_FACE('',(#1269),#4473,.T.);
#4646=ADVANCED_FACE('',(#1270,#1123,#1124,#1125,#1126,#1127,#1128,#1129,
#1130),#4474,.T.);
#4647=ADVANCED_FACE('',(#1271,#1131,#1132,#1133,#1134),#4475,.F.);
#4648=ADVANCED_FACE('',(#1272),#1026,.F.);
#4649=ADVANCED_FACE('',(#1273),#1027,.F.);
#4650=ADVANCED_FACE('',(#1274),#1028,.F.);
#4651=ADVANCED_FACE('',(#1275,#1135,#1136),#4476,.T.);
#4652=ADVANCED_FACE('',(#1276),#4477,.T.);
#4653=ADVANCED_FACE('',(#1277,#1137,#1138),#4478,.T.);
#4654=ADVANCED_FACE('',(#1278),#4479,.T.);
#4655=ADVANCED_FACE('',(#1279,#1139),#4480,.T.);
#4656=ADVANCED_FACE('',(#1280,#1140),#4481,.F.);
#4657=ADVANCED_FACE('',(#1281),#1029,.F.);
#4658=ADVANCED_FACE('',(#1282),#1030,.T.);
#4659=ADVANCED_FACE('',(#1283,#1141),#4482,.T.);
#4660=ADVANCED_FACE('',(#1284,#1142),#4483,.F.);
#4661=ADVANCED_FACE('',(#1285),#1031,.F.);
#4662=ADVANCED_FACE('',(#1286),#4484,.T.);
#4663=ADVANCED_FACE('',(#1287,#1143),#4485,.T.);
#4664=ADVANCED_FACE('',(#1288),#1032,.T.);
#4665=ADVANCED_FACE('',(#1289),#4486,.F.);
#4666=ADVANCED_FACE('',(#1290),#1033,.T.);
#4667=ADVANCED_FACE('',(#1291,#1144),#4487,.T.);
#4668=ADVANCED_FACE('',(#1292),#1034,.F.);
#4669=ADVANCED_FACE('',(#1293),#1035,.T.);
#4670=ADVANCED_FACE('',(#1294,#1145),#4488,.T.);
#4671=ADVANCED_FACE('',(#1295,#1146),#4489,.F.);
#4672=ADVANCED_FACE('',(#1296),#1036,.F.);
#4673=ADVANCED_FACE('',(#1297),#1037,.T.);
#4674=ADVANCED_FACE('',(#1298,#1147),#4490,.T.);
#4675=ADVANCED_FACE('',(#1299,#1148),#4491,.F.);
#4676=ADVANCED_FACE('',(#1300),#1038,.F.);
#4677=ADVANCED_FACE('',(#1301),#1039,.T.);
#4678=ADVANCED_FACE('',(#1302,#1149),#4492,.T.);
#4679=ADVANCED_FACE('',(#1303,#1150),#4493,.F.);
#4680=ADVANCED_FACE('',(#1304),#1040,.F.);
#4681=ADVANCED_FACE('',(#1305),#1041,.T.);
#4682=ADVANCED_FACE('',(#1306,#1151),#4494,.T.);
#4683=ADVANCED_FACE('',(#1307,#1152),#4495,.F.);
#4684=ADVANCED_FACE('',(#1308),#1042,.F.);
#4685=ADVANCED_FACE('',(#1309),#1043,.T.);
#4686=ADVANCED_FACE('',(#1310,#1153),#4496,.T.);
#4687=ADVANCED_FACE('',(#1311,#1154),#4497,.F.);
#4688=ADVANCED_FACE('',(#1312),#1044,.F.);
#4689=ADVANCED_FACE('',(#1313),#1045,.T.);
#4690=ADVANCED_FACE('',(#1314,#1155),#4498,.T.);
#4691=ADVANCED_FACE('',(#1315,#1156),#4499,.F.);
#4692=ADVANCED_FACE('',(#1316),#1046,.F.);
#4693=ADVANCED_FACE('',(#1317),#1047,.T.);
#4694=ADVANCED_FACE('',(#1318,#1157),#4500,.T.);
#4695=ADVANCED_FACE('',(#1319,#1158),#4501,.F.);
#4696=ADVANCED_FACE('',(#1320),#4502,.F.);
#4697=ADVANCED_FACE('',(#1321),#4503,.F.);
#4698=ADVANCED_FACE('',(#1322),#4504,.F.);
#4699=ADVANCED_FACE('',(#1323),#4505,.F.);
#4700=ADVANCED_FACE('',(#1324),#4506,.F.);
#4701=ADVANCED_FACE('',(#1325),#4507,.F.);
#4702=ADVANCED_FACE('',(#1326),#4508,.F.);
#4703=ADVANCED_FACE('',(#1327),#4509,.F.);
#4704=ADVANCED_FACE('',(#1328,#1159),#4510,.T.);
#4705=ADVANCED_FACE('',(#1329),#1048,.T.);
#4706=ADVANCED_FACE('',(#1330),#4511,.F.);
#4707=ADVANCED_FACE('',(#1331),#4512,.T.);
#4708=ADVANCED_FACE('',(#1332),#267,.T.);
#4709=ADVANCED_FACE('',(#1333),#1049,.T.);
#4710=ADVANCED_FACE('',(#1334),#268,.T.);
#4711=ADVANCED_FACE('',(#1335,#1160),#4513,.T.);
#4712=ADVANCED_FACE('',(#1336),#269,.T.);
#4713=ADVANCED_FACE('',(#1337),#1050,.T.);
#4714=ADVANCED_FACE('',(#1338),#1051,.F.);
#4715=ADVANCED_FACE('',(#1339),#1052,.T.);
#4716=ADVANCED_FACE('',(#1340,#1161),#4514,.T.);
#4717=ADVANCED_FACE('',(#1341,#1162),#4515,.F.);
#4718=ADVANCED_FACE('',(#1342),#270,.T.);
#4719=ADVANCED_FACE('',(#1343),#271,.T.);
#4720=ADVANCED_FACE('',(#1344),#4516,.T.);
#4721=ADVANCED_FACE('',(#1345),#4517,.T.);
#4722=ADVANCED_FACE('',(#1346),#4518,.T.);
#4723=ADVANCED_FACE('',(#1347),#1053,.F.);
#4724=ADVANCED_FACE('',(#1348),#4519,.T.);
#4725=ADVANCED_FACE('',(#1349),#4520,.T.);
#4726=ADVANCED_FACE('',(#1350),#4521,.T.);
#4727=ADVANCED_FACE('',(#1351,#1163),#4522,.T.);
#4728=ADVANCED_FACE('',(#1352,#1164),#4523,.F.);
#4729=ADVANCED_FACE('',(#1353),#4524,.T.);
#4730=ADVANCED_FACE('',(#1354),#272,.T.);
#4731=ADVANCED_FACE('',(#1355),#1054,.T.);
#4732=ADVANCED_FACE('',(#1356),#273,.T.);
#4733=ADVANCED_FACE('',(#1357,#1165),#4525,.T.);
#4734=ADVANCED_FACE('',(#1358),#274,.T.);
#4735=ADVANCED_FACE('',(#1359),#1055,.T.);
#4736=ADVANCED_FACE('',(#1360),#275,.T.);
#4737=ADVANCED_FACE('',(#1361),#4526,.T.);
#4738=ADVANCED_FACE('',(#1362),#4527,.F.);
#4739=ADVANCED_FACE('',(#1363),#4528,.F.);
#4740=ADVANCED_FACE('',(#1364),#4529,.F.);
#4741=ADVANCED_FACE('',(#1365),#4530,.F.);
#4742=ADVANCED_FACE('',(#1366),#4531,.F.);
#4743=ADVANCED_FACE('',(#1367),#4532,.F.);
#4744=ADVANCED_FACE('',(#1368),#4533,.F.);
#4745=ADVANCED_FACE('',(#1369),#4534,.F.);
#4746=ADVANCED_FACE('',(#1370),#1056,.F.);
#4747=ADVANCED_FACE('',(#1371),#1057,.F.);
#4748=ADVANCED_FACE('',(#1372),#1058,.F.);
#4749=ADVANCED_FACE('',(#1373),#1059,.F.);
#4750=ADVANCED_FACE('',(#1374),#276,.T.);
#4751=ADVANCED_FACE('',(#1375),#277,.T.);
#4752=ADVANCED_FACE('',(#1376),#1060,.T.);
#4753=ADVANCED_FACE('',(#1377,#1166),#4535,.T.);
#4754=ADVANCED_FACE('',(#1378,#1167),#4536,.F.);
#4755=ADVANCED_FACE('',(#1379),#1061,.T.);
#4756=ADVANCED_FACE('',(#1380),#1062,.T.);
#4757=ADVANCED_FACE('',(#1381),#1063,.F.);
#4758=ADVANCED_FACE('',(#1382),#1064,.T.);
#4759=ADVANCED_FACE('',(#1383,#1168,#1169,#1170,#1171,#1172),#4537,.T.);
#4760=ADVANCED_FACE('',(#1384,#1173,#1174,#1175,#1176,#1177),#4538,.F.);
#4761=ADVANCED_FACE('',(#1385),#1065,.F.);
#4762=ADVANCED_FACE('',(#1386),#1066,.T.);
#4763=ADVANCED_FACE('',(#1387,#1178),#4539,.T.);
#4764=ADVANCED_FACE('',(#1388,#1179),#4540,.F.);
#4765=ADVANCED_FACE('',(#1389),#1067,.F.);
#4766=ADVANCED_FACE('',(#1390),#1068,.F.);
#4767=ADVANCED_FACE('',(#1391),#1069,.F.);
#4768=ADVANCED_FACE('',(#1392),#1070,.F.);
#4769=ADVANCED_FACE('',(#1393),#1071,.T.);
#4770=ADVANCED_FACE('',(#1394,#1180),#4541,.T.);
#4771=ADVANCED_FACE('',(#1395),#1072,.F.);
#4772=ADVANCED_FACE('',(#1396),#1073,.T.);
#4773=ADVANCED_FACE('',(#1397,#1181,#1182,#1183,#1184,#1185),#4542,.T.);
#4774=ADVANCED_FACE('',(#1398,#1186,#1187,#1188,#1189,#1190),#4543,.F.);
#4775=ADVANCED_FACE('',(#1399),#1074,.F.);
#4776=ADVANCED_FACE('',(#1400),#1075,.F.);
#4777=ADVANCED_FACE('',(#1401),#1076,.F.);
#4778=ADVANCED_FACE('',(#1402),#1077,.F.);
#4779=ADVANCED_FACE('',(#1403),#1078,.T.);
#4780=ADVANCED_FACE('',(#1404,#1191),#4544,.F.);
#4781=ADVANCED_FACE('',(#1405),#1079,.F.);
#4782=ADVANCED_FACE('',(#1406),#1080,.T.);
#4783=ADVANCED_FACE('',(#1407,#1192,#1193,#1194,#1195,#1196),#4545,.T.);
#4784=ADVANCED_FACE('',(#1408,#1197,#1198,#1199,#1200,#1201),#4546,.F.);
#4785=ADVANCED_FACE('',(#1409),#45,.F.);
#4786=ADVANCED_FACE('',(#1410),#1081,.T.);
#4787=ADVANCED_FACE('',(#1411),#1082,.F.);
#4788=ADVANCED_FACE('',(#1412),#278,.F.);
#4789=ADVANCED_FACE('',(#1413,#1202),#4547,.T.);
#4790=ADVANCED_FACE('',(#1414),#1083,.T.);
#4791=ADVANCED_FACE('',(#1415,#1203),#4548,.T.);
#4792=ADVANCED_FACE('',(#1416),#279,.F.);
#4793=ADVANCED_FACE('',(#1417),#46,.F.);
#4794=ADVANCED_FACE('',(#1418),#1084,.F.);
#4795=ADVANCED_FACE('',(#1419,#1204),#4549,.T.);
#4796=ADVANCED_FACE('',(#1420),#280,.T.);
#4797=ADVANCED_FACE('',(#1421),#1085,.T.);
#4798=ADVANCED_FACE('',(#1422),#281,.T.);
#4799=ADVANCED_FACE('',(#1423,#1205),#4550,.T.);
#4800=ADVANCED_FACE('',(#1424),#1086,.F.);
#4801=ADVANCED_FACE('',(#1425),#29,.T.);
#4802=ADVANCED_FACE('',(#1426),#30,.T.);
#4803=ADVANCED_FACE('',(#1427),#31,.T.);
#4804=ADVANCED_FACE('',(#1428),#32,.T.);
#4805=ADVANCED_FACE('',(#1429),#33,.T.);
#4806=ADVANCED_FACE('',(#1430),#34,.T.);
#4807=ADVANCED_FACE('',(#1431),#35,.T.);
#4808=ADVANCED_FACE('',(#1432),#36,.T.);
#4809=ADVANCED_FACE('',(#1433),#37,.F.);
#4810=ADVANCED_FACE('',(#1434),#1087,.T.);
#4811=ADVANCED_FACE('',(#1435),#4551,.T.);
#4812=ADVANCED_FACE('',(#1436),#38,.F.);
#4813=ADVANCED_FACE('',(#1437),#4552,.T.);
#4814=ADVANCED_FACE('',(#1438),#39,.F.);
#4815=ADVANCED_FACE('',(#1439),#4553,.T.);
#4816=ADVANCED_FACE('',(#1440),#40,.F.);
#4817=ADVANCED_FACE('',(#1441),#4554,.T.);
#4818=ADVANCED_FACE('',(#1442),#41,.F.);
#4819=ADVANCED_FACE('',(#1443),#4555,.T.);
#4820=ADVANCED_FACE('',(#1444),#42,.F.);
#4821=ADVANCED_FACE('',(#1445),#4556,.T.);
#4822=ADVANCED_FACE('',(#1446),#43,.F.);
#4823=ADVANCED_FACE('',(#1447),#1088,.F.);
#4824=ADVANCED_FACE('',(#1448),#4557,.T.);
#4825=ADVANCED_FACE('',(#1449),#44,.F.);
#4826=ADVANCED_FACE('',(#1450,#1206),#4558,.T.);
#4827=ADVANCED_FACE('',(#1451),#4559,.T.);
#4828=ADVANCED_FACE('',(#1452,#1207),#4560,.T.);
#4829=ADVANCED_FACE('',(#1453),#1089,.T.);
#4830=ADVANCED_FACE('',(#1454,#1208),#4561,.T.);
#4831=ADVANCED_FACE('',(#1455),#1090,.F.);
#4832=ADVANCED_FACE('',(#1456,#1209),#4562,.T.);
#4833=ADVANCED_FACE('',(#1457),#1091,.T.);
#4834=ADVANCED_FACE('',(#1458,#1210),#4563,.T.);
#4835=ADVANCED_FACE('',(#1459),#1092,.F.);
#4836=ADVANCED_FACE('',(#1460),#4564,.F.);
#4837=ADVANCED_FACE('',(#1461),#4565,.F.);
#4838=ADVANCED_FACE('',(#1462),#4566,.F.);
#4839=ADVANCED_FACE('',(#1463),#4567,.F.);
#4840=ADVANCED_FACE('',(#1464),#4568,.F.);
#4841=ADVANCED_FACE('',(#1465),#4569,.F.);
#4842=ADVANCED_FACE('',(#1466),#4570,.F.);
#4843=ADVANCED_FACE('',(#1467),#4571,.F.);
#4844=ADVANCED_FACE('',(#1468),#4572,.F.);
#4845=ADVANCED_FACE('',(#1469),#4573,.T.);
#4846=ADVANCED_FACE('',(#1470),#282,.T.);
#4847=ADVANCED_FACE('',(#1471),#1093,.T.);
#4848=ADVANCED_FACE('',(#1472),#283,.T.);
#4849=ADVANCED_FACE('',(#1473,#1211),#4574,.T.);
#4850=ADVANCED_FACE('',(#1474),#284,.T.);
#4851=ADVANCED_FACE('',(#1475),#1094,.T.);
#4852=ADVANCED_FACE('',(#1476,#1212),#4575,.T.);
#4853=ADVANCED_FACE('',(#1477,#1213),#4576,.F.);
#4854=ADVANCED_FACE('',(#1478),#1095,.T.);
#4855=ADVANCED_FACE('',(#1479),#1096,.T.);
#4856=ADVANCED_FACE('',(#1480),#1097,.T.);
#4857=ADVANCED_FACE('',(#1481),#4577,.T.);
#4858=ADVANCED_FACE('',(#1482),#4578,.T.);
#4859=ADVANCED_FACE('',(#1483),#4579,.T.);
#4860=ADVANCED_FACE('',(#1484),#4580,.T.);
#4861=ADVANCED_FACE('',(#1485),#4581,.T.);
#4862=ADVANCED_FACE('',(#1486),#4582,.T.);
#4863=ADVANCED_FACE('',(#1487),#1098,.F.);
#4864=ADVANCED_FACE('',(#1488),#4583,.F.);
#4865=ADVANCED_FACE('',(#1489),#4584,.F.);
#4866=ADVANCED_FACE('',(#1490),#4585,.F.);
#4867=ADVANCED_FACE('',(#1491),#1099,.T.);
#4868=ADVANCED_FACE('',(#1492),#1100,.F.);
#4869=ADVANCED_FACE('',(#1493),#1101,.T.);
#4870=ADVANCED_FACE('',(#1494,#1214),#4586,.T.);
#4871=ADVANCED_FACE('',(#1495,#1215),#4587,.F.);
#4872=ADVANCED_FACE('',(#1496),#1102,.F.);
#4873=ADVANCED_FACE('',(#1497),#4588,.T.);
#4874=ADVANCED_FACE('',(#1498),#4589,.T.);
#4875=ADVANCED_FACE('',(#1499),#4590,.T.);
#4876=ADVANCED_FACE('',(#1500),#4591,.T.);
#4877=ADVANCED_FACE('',(#1501),#4592,.T.);
#4878=ADVANCED_FACE('',(#1502),#4593,.T.);
#4879=ADVANCED_FACE('',(#1503,#1216),#4594,.T.);
#4880=ADVANCED_FACE('',(#1504,#1217),#4595,.F.);
#4881=ADVANCED_FACE('',(#1505),#1103,.F.);
#4882=ADVANCED_FACE('',(#1506),#1104,.F.);
#4883=ADVANCED_FACE('',(#1507),#1105,.T.);
#4884=ADVANCED_FACE('',(#1508,#1218,#1219),#4596,.T.);
#4885=ADVANCED_FACE('',(#1509),#1106,.T.);
#4886=ADVANCED_FACE('',(#1510,#1220,#1221),#4597,.F.);
#4887=CLOSED_SHELL('',(#4598,#4599,#4600,#4601,#4602,#4603,#4604,#4605,
#4606,#4607,#4608,#4609,#4610,#4611,#4612,#4613,#4614,#4615,#4616,#4617,
#4618,#4619,#4620,#4621,#4622));
#4888=CLOSED_SHELL('',(#4623,#4624,#4625,#4626,#4627,#4628,#4629,#4630,
#4631,#4632,#4633,#4634,#4635,#4636,#4637,#4638,#4639,#4640,#4641,#4642,
#4643,#4644,#4645,#4646,#4647));
#4889=CLOSED_SHELL('',(#4648,#4649,#4650,#4651,#4652,#4653,#4654,#4655,
#4656));
#4890=CLOSED_SHELL('',(#4657,#4658,#4659,#4660));
#4891=CLOSED_SHELL('',(#4661,#4662,#4663,#4664,#4665,#4666,#4667));
#4892=CLOSED_SHELL('',(#4668,#4669,#4670,#4671));
#4893=CLOSED_SHELL('',(#4672,#4673,#4674,#4675));
#4894=CLOSED_SHELL('',(#4676,#4677,#4678,#4679));
#4895=CLOSED_SHELL('',(#4680,#4681,#4682,#4683));
#4896=CLOSED_SHELL('',(#4684,#4685,#4686,#4687));
#4897=CLOSED_SHELL('',(#4688,#4689,#4690,#4691));
#4898=CLOSED_SHELL('',(#4692,#4693,#4694,#4695));
#4899=CLOSED_SHELL('',(#4696,#4697,#4698,#4699,#4700,#4701,#4702,#4703));
#4900=CLOSED_SHELL('',(#4704,#4705,#4706,#4707,#4708,#4709,#4710,#4711,
#4712,#4713));
#4901=CLOSED_SHELL('',(#4714,#4715,#4716,#4717));
#4902=CLOSED_SHELL('',(#4718,#4719,#4720,#4721,#4722,#4723,#4724,#4725,
#4726,#4727,#4728));
#4903=CLOSED_SHELL('',(#4729,#4730,#4731,#4732,#4733,#4734,#4735,#4736,
#4737));
#4904=CLOSED_SHELL('',(#4738,#4739,#4740,#4741,#4742,#4743,#4744,#4745));
#4905=CLOSED_SHELL('',(#4746,#4747,#4748,#4749,#4750,#4751,#4752,#4753,
#4754,#4755,#4756,#4757,#4758,#4759,#4760));
#4906=CLOSED_SHELL('',(#4761,#4762,#4763,#4764));
#4907=CLOSED_SHELL('',(#4765,#4766,#4767,#4768,#4769,#4770,#4771,#4772,
#4773,#4774));
#4908=CLOSED_SHELL('',(#4775,#4776,#4777,#4778,#4779,#4780,#4781,#4782,
#4783,#4784));
#4909=CLOSED_SHELL('',(#4785,#4786,#4787,#4788,#4789,#4790,#4791,#4792));
#4910=CLOSED_SHELL('',(#4793,#4794,#4795,#4796,#4797,#4798,#4799,#4800));
#4911=CLOSED_SHELL('',(#4801));
#4912=CLOSED_SHELL('',(#4802));
#4913=CLOSED_SHELL('',(#4803));
#4914=CLOSED_SHELL('',(#4804));
#4915=CLOSED_SHELL('',(#4805));
#4916=CLOSED_SHELL('',(#4806));
#4917=CLOSED_SHELL('',(#4807));
#4918=CLOSED_SHELL('',(#4808));
#4919=CLOSED_SHELL('',(#4809,#4810,#4811,#4812,#4813,#4814,#4815,#4816,
#4817,#4818,#4819,#4820,#4821,#4822,#4823,#4824,#4825,#4826,#4827));
#4920=CLOSED_SHELL('',(#4828,#4829,#4830,#4831));
#4921=CLOSED_SHELL('',(#4832,#4833,#4834,#4835));
#4922=CLOSED_SHELL('',(#4836,#4837,#4838,#4839,#4840,#4841,#4842,#4843));
#4923=CLOSED_SHELL('',(#4844,#4845,#4846,#4847,#4848,#4849,#4850,#4851));
#4924=CLOSED_SHELL('',(#4852,#4853,#4854,#4855,#4856,#4857,#4858,#4859,
#4860,#4861,#4862,#4863,#4864,#4865,#4866,#4867));
#4925=CLOSED_SHELL('',(#4868,#4869,#4870,#4871));
#4926=CLOSED_SHELL('',(#4872,#4873,#4874,#4875,#4876,#4877,#4878,#4879,
#4880));
#4927=CLOSED_SHELL('',(#4881,#4882,#4883,#4884,#4885,#4886));
#4928=DERIVED_UNIT_ELEMENT(#4988,1.);
#4929=DERIVED_UNIT_ELEMENT(#9393,-3.);
#4930=DERIVED_UNIT_ELEMENT(#4988,1.);
#4931=DERIVED_UNIT_ELEMENT(#9393,-3.);
#4932=DERIVED_UNIT_ELEMENT(#4988,1.);
#4933=DERIVED_UNIT_ELEMENT(#9393,-3.);
#4934=DERIVED_UNIT_ELEMENT(#4988,1.);
#4935=DERIVED_UNIT_ELEMENT(#9393,-3.);
#4936=DERIVED_UNIT_ELEMENT(#4988,1.);
#4937=DERIVED_UNIT_ELEMENT(#9393,-3.);
#4938=DERIVED_UNIT_ELEMENT(#4988,1.);
#4939=DERIVED_UNIT_ELEMENT(#9393,-3.);
#4940=DERIVED_UNIT_ELEMENT(#4988,1.);
#4941=DERIVED_UNIT_ELEMENT(#9393,-3.);
#4942=DERIVED_UNIT_ELEMENT(#4988,1.);
#4943=DERIVED_UNIT_ELEMENT(#9393,-3.);
#4944=DERIVED_UNIT_ELEMENT(#4988,1.);
#4945=DERIVED_UNIT_ELEMENT(#9393,-3.);
#4946=DERIVED_UNIT_ELEMENT(#4988,1.);
#4947=DERIVED_UNIT_ELEMENT(#9393,-3.);
#4948=DERIVED_UNIT_ELEMENT(#4988,1.);
#4949=DERIVED_UNIT_ELEMENT(#9393,-3.);
#4950=DERIVED_UNIT_ELEMENT(#4988,1.);
#4951=DERIVED_UNIT_ELEMENT(#9393,-3.);
#4952=DERIVED_UNIT_ELEMENT(#4988,1.);
#4953=DERIVED_UNIT_ELEMENT(#9393,-3.);
#4954=DERIVED_UNIT_ELEMENT(#4988,1.);
#4955=DERIVED_UNIT_ELEMENT(#9393,-3.);
#4956=DERIVED_UNIT_ELEMENT(#4988,1.);
#4957=DERIVED_UNIT_ELEMENT(#9393,-3.);
#4958=DERIVED_UNIT_ELEMENT(#4988,1.);
#4959=DERIVED_UNIT_ELEMENT(#9393,-3.);
#4960=DERIVED_UNIT_ELEMENT(#4988,1.);
#4961=DERIVED_UNIT_ELEMENT(#9393,-3.);
#4962=DERIVED_UNIT_ELEMENT(#4988,1.);
#4963=DERIVED_UNIT_ELEMENT(#9393,-3.);
#4964=DERIVED_UNIT_ELEMENT(#4988,1.);
#4965=DERIVED_UNIT_ELEMENT(#9393,-3.);
#4966=DERIVED_UNIT_ELEMENT(#4988,1.);
#4967=DERIVED_UNIT_ELEMENT(#9393,-3.);
#4968=DERIVED_UNIT_ELEMENT(#4988,1.);
#4969=DERIVED_UNIT_ELEMENT(#9393,-3.);
#4970=DERIVED_UNIT_ELEMENT(#4988,1.);
#4971=DERIVED_UNIT_ELEMENT(#9393,-3.);
#4972=DERIVED_UNIT_ELEMENT(#4988,1.);
#4973=DERIVED_UNIT_ELEMENT(#9393,-3.);
#4974=DERIVED_UNIT_ELEMENT(#4988,1.);
#4975=DERIVED_UNIT_ELEMENT(#9393,-3.);
#4976=DERIVED_UNIT_ELEMENT(#4988,1.);
#4977=DERIVED_UNIT_ELEMENT(#9393,-3.);
#4978=DERIVED_UNIT_ELEMENT(#4988,1.);
#4979=DERIVED_UNIT_ELEMENT(#9393,-3.);
#4980=DERIVED_UNIT_ELEMENT(#4988,1.);
#4981=DERIVED_UNIT_ELEMENT(#9393,-3.);
#4982=DERIVED_UNIT_ELEMENT(#4988,1.);
#4983=DERIVED_UNIT_ELEMENT(#9393,-3.);
#4984=DERIVED_UNIT_ELEMENT(#4988,1.);
#4985=DERIVED_UNIT_ELEMENT(#9393,-3.);
#4986=DERIVED_UNIT_ELEMENT(#4988,1.);
#4987=DERIVED_UNIT_ELEMENT(#9393,-3.);
#4988=(
MASS_UNIT()
NAMED_UNIT(*)
SI_UNIT(.KILO.,.GRAM.)
);
#4989=DERIVED_UNIT((#4928,#4929));
#4990=DERIVED_UNIT((#4930,#4931));
#4991=DERIVED_UNIT((#4932,#4933));
#4992=DERIVED_UNIT((#4934,#4935));
#4993=DERIVED_UNIT((#4936,#4937));
#4994=DERIVED_UNIT((#4938,#4939));
#4995=DERIVED_UNIT((#4940,#4941));
#4996=DERIVED_UNIT((#4942,#4943));
#4997=DERIVED_UNIT((#4944,#4945));
#4998=DERIVED_UNIT((#4946,#4947));
#4999=DERIVED_UNIT((#4948,#4949));
#5000=DERIVED_UNIT((#4950,#4951));
#5001=DERIVED_UNIT((#4952,#4953));
#5002=DERIVED_UNIT((#4954,#4955));
#5003=DERIVED_UNIT((#4956,#4957));
#5004=DERIVED_UNIT((#4958,#4959));
#5005=DERIVED_UNIT((#4960,#4961));
#5006=DERIVED_UNIT((#4962,#4963));
#5007=DERIVED_UNIT((#4964,#4965));
#5008=DERIVED_UNIT((#4966,#4967));
#5009=DERIVED_UNIT((#4968,#4969));
#5010=DERIVED_UNIT((#4970,#4971));
#5011=DERIVED_UNIT((#4972,#4973));
#5012=DERIVED_UNIT((#4974,#4975));
#5013=DERIVED_UNIT((#4976,#4977));
#5014=DERIVED_UNIT((#4978,#4979));
#5015=DERIVED_UNIT((#4980,#4981));
#5016=DERIVED_UNIT((#4982,#4983));
#5017=DERIVED_UNIT((#4984,#4985));
#5018=DERIVED_UNIT((#4986,#4987));
#5019=MEASURE_REPRESENTATION_ITEM('density measure',
POSITIVE_RATIO_MEASURE(7850.),#4989);
#5020=MEASURE_REPRESENTATION_ITEM('density measure',
POSITIVE_RATIO_MEASURE(7850.),#4990);
#5021=MEASURE_REPRESENTATION_ITEM('density measure',
POSITIVE_RATIO_MEASURE(7850.),#4991);
#5022=MEASURE_REPRESENTATION_ITEM('density measure',
POSITIVE_RATIO_MEASURE(7850.),#4992);
#5023=MEASURE_REPRESENTATION_ITEM('density measure',
POSITIVE_RATIO_MEASURE(7850.),#4993);
#5024=MEASURE_REPRESENTATION_ITEM('density measure',
POSITIVE_RATIO_MEASURE(7850.),#4994);
#5025=MEASURE_REPRESENTATION_ITEM('density measure',
POSITIVE_RATIO_MEASURE(7850.),#4995);
#5026=MEASURE_REPRESENTATION_ITEM('density measure',
POSITIVE_RATIO_MEASURE(7850.),#4996);
#5027=MEASURE_REPRESENTATION_ITEM('density measure',
POSITIVE_RATIO_MEASURE(7850.),#4997);
#5028=MEASURE_REPRESENTATION_ITEM('density measure',
POSITIVE_RATIO_MEASURE(7850.),#4998);
#5029=MEASURE_REPRESENTATION_ITEM('density measure',
POSITIVE_RATIO_MEASURE(7850.),#4999);
#5030=MEASURE_REPRESENTATION_ITEM('density measure',
POSITIVE_RATIO_MEASURE(7850.),#5000);
#5031=MEASURE_REPRESENTATION_ITEM('density measure',
POSITIVE_RATIO_MEASURE(7850.),#5001);
#5032=MEASURE_REPRESENTATION_ITEM('density measure',
POSITIVE_RATIO_MEASURE(7850.),#5002);
#5033=MEASURE_REPRESENTATION_ITEM('density measure',
POSITIVE_RATIO_MEASURE(7850.),#5003);
#5034=MEASURE_REPRESENTATION_ITEM('density measure',
POSITIVE_RATIO_MEASURE(7850.),#5004);
#5035=MEASURE_REPRESENTATION_ITEM('density measure',
POSITIVE_RATIO_MEASURE(7850.),#5005);
#5036=MEASURE_REPRESENTATION_ITEM('density measure',
POSITIVE_RATIO_MEASURE(7850.),#5006);
#5037=MEASURE_REPRESENTATION_ITEM('density measure',
POSITIVE_RATIO_MEASURE(7850.),#5007);
#5038=MEASURE_REPRESENTATION_ITEM('density measure',
POSITIVE_RATIO_MEASURE(7850.),#5008);
#5039=MEASURE_REPRESENTATION_ITEM('density measure',
POSITIVE_RATIO_MEASURE(7850.),#5009);
#5040=MEASURE_REPRESENTATION_ITEM('density measure',
POSITIVE_RATIO_MEASURE(7850.),#5010);
#5041=MEASURE_REPRESENTATION_ITEM('density measure',
POSITIVE_RATIO_MEASURE(7850.),#5011);
#5042=MEASURE_REPRESENTATION_ITEM('density measure',
POSITIVE_RATIO_MEASURE(7850.),#5012);
#5043=MEASURE_REPRESENTATION_ITEM('density measure',
POSITIVE_RATIO_MEASURE(7850.),#5013);
#5044=MEASURE_REPRESENTATION_ITEM('density measure',
POSITIVE_RATIO_MEASURE(7850.),#5014);
#5045=MEASURE_REPRESENTATION_ITEM('density measure',
POSITIVE_RATIO_MEASURE(7850.),#5015);
#5046=MEASURE_REPRESENTATION_ITEM('density measure',
POSITIVE_RATIO_MEASURE(7850.),#5016);
#5047=MEASURE_REPRESENTATION_ITEM('density measure',
POSITIVE_RATIO_MEASURE(7850.),#5017);
#5048=MEASURE_REPRESENTATION_ITEM('density measure',
POSITIVE_RATIO_MEASURE(7850.),#5018);
#5049=PROPERTY_DEFINITION_REPRESENTATION(#5199,#5109);
#5050=PROPERTY_DEFINITION_REPRESENTATION(#5200,#5110);
#5051=PROPERTY_DEFINITION_REPRESENTATION(#5201,#5111);
#5052=PROPERTY_DEFINITION_REPRESENTATION(#5202,#5112);
#5053=PROPERTY_DEFINITION_REPRESENTATION(#5203,#5113);
#5054=PROPERTY_DEFINITION_REPRESENTATION(#5204,#5114);
#5055=PROPERTY_DEFINITION_REPRESENTATION(#5205,#5115);
#5056=PROPERTY_DEFINITION_REPRESENTATION(#5206,#5116);
#5057=PROPERTY_DEFINITION_REPRESENTATION(#5207,#5117);
#5058=PROPERTY_DEFINITION_REPRESENTATION(#5208,#5118);
#5059=PROPERTY_DEFINITION_REPRESENTATION(#5209,#5119);
#5060=PROPERTY_DEFINITION_REPRESENTATION(#5210,#5120);
#5061=PROPERTY_DEFINITION_REPRESENTATION(#5211,#5121);
#5062=PROPERTY_DEFINITION_REPRESENTATION(#5212,#5122);
#5063=PROPERTY_DEFINITION_REPRESENTATION(#5213,#5123);
#5064=PROPERTY_DEFINITION_REPRESENTATION(#5214,#5124);
#5065=PROPERTY_DEFINITION_REPRESENTATION(#5215,#5125);
#5066=PROPERTY_DEFINITION_REPRESENTATION(#5216,#5126);
#5067=PROPERTY_DEFINITION_REPRESENTATION(#5217,#5127);
#5068=PROPERTY_DEFINITION_REPRESENTATION(#5218,#5128);
#5069=PROPERTY_DEFINITION_REPRESENTATION(#5219,#5129);
#5070=PROPERTY_DEFINITION_REPRESENTATION(#5220,#5130);
#5071=PROPERTY_DEFINITION_REPRESENTATION(#5221,#5131);
#5072=PROPERTY_DEFINITION_REPRESENTATION(#5222,#5132);
#5073=PROPERTY_DEFINITION_REPRESENTATION(#5223,#5133);
#5074=PROPERTY_DEFINITION_REPRESENTATION(#5224,#5134);
#5075=PROPERTY_DEFINITION_REPRESENTATION(#5225,#5135);
#5076=PROPERTY_DEFINITION_REPRESENTATION(#5226,#5136);
#5077=PROPERTY_DEFINITION_REPRESENTATION(#5227,#5137);
#5078=PROPERTY_DEFINITION_REPRESENTATION(#5228,#5138);
#5079=PROPERTY_DEFINITION_REPRESENTATION(#5229,#5139);
#5080=PROPERTY_DEFINITION_REPRESENTATION(#5230,#5140);
#5081=PROPERTY_DEFINITION_REPRESENTATION(#5231,#5141);
#5082=PROPERTY_DEFINITION_REPRESENTATION(#5232,#5142);
#5083=PROPERTY_DEFINITION_REPRESENTATION(#5233,#5143);
#5084=PROPERTY_DEFINITION_REPRESENTATION(#5234,#5144);
#5085=PROPERTY_DEFINITION_REPRESENTATION(#5235,#5145);
#5086=PROPERTY_DEFINITION_REPRESENTATION(#5236,#5146);
#5087=PROPERTY_DEFINITION_REPRESENTATION(#5237,#5147);
#5088=PROPERTY_DEFINITION_REPRESENTATION(#5238,#5148);
#5089=PROPERTY_DEFINITION_REPRESENTATION(#5239,#5149);
#5090=PROPERTY_DEFINITION_REPRESENTATION(#5240,#5150);
#5091=PROPERTY_DEFINITION_REPRESENTATION(#5241,#5151);
#5092=PROPERTY_DEFINITION_REPRESENTATION(#5242,#5152);
#5093=PROPERTY_DEFINITION_REPRESENTATION(#5243,#5153);
#5094=PROPERTY_DEFINITION_REPRESENTATION(#5244,#5154);
#5095=PROPERTY_DEFINITION_REPRESENTATION(#5245,#5155);
#5096=PROPERTY_DEFINITION_REPRESENTATION(#5246,#5156);
#5097=PROPERTY_DEFINITION_REPRESENTATION(#5247,#5157);
#5098=PROPERTY_DEFINITION_REPRESENTATION(#5248,#5158);
#5099=PROPERTY_DEFINITION_REPRESENTATION(#5249,#5159);
#5100=PROPERTY_DEFINITION_REPRESENTATION(#5250,#5160);
#5101=PROPERTY_DEFINITION_REPRESENTATION(#5251,#5161);
#5102=PROPERTY_DEFINITION_REPRESENTATION(#5252,#5162);
#5103=PROPERTY_DEFINITION_REPRESENTATION(#5253,#5163);
#5104=PROPERTY_DEFINITION_REPRESENTATION(#5254,#5164);
#5105=PROPERTY_DEFINITION_REPRESENTATION(#5255,#5165);
#5106=PROPERTY_DEFINITION_REPRESENTATION(#5256,#5166);
#5107=PROPERTY_DEFINITION_REPRESENTATION(#5257,#5167);
#5108=PROPERTY_DEFINITION_REPRESENTATION(#5258,#5168);
#5109=REPRESENTATION('material name',(#5169),#9357);
#5110=REPRESENTATION('density',(#5019),#9357);
#5111=REPRESENTATION('material name',(#5170),#9358);
#5112=REPRESENTATION('density',(#5020),#9358);
#5113=REPRESENTATION('material name',(#5171),#9359);
#5114=REPRESENTATION('density',(#5021),#9359);
#5115=REPRESENTATION('material name',(#5172),#9360);
#5116=REPRESENTATION('density',(#5022),#9360);
#5117=REPRESENTATION('material name',(#5173),#9361);
#5118=REPRESENTATION('density',(#5023),#9361);
#5119=REPRESENTATION('material name',(#5174),#9362);
#5120=REPRESENTATION('density',(#5024),#9362);
#5121=REPRESENTATION('material name',(#5175),#9363);
#5122=REPRESENTATION('density',(#5025),#9363);
#5123=REPRESENTATION('material name',(#5176),#9364);
#5124=REPRESENTATION('density',(#5026),#9364);
#5125=REPRESENTATION('material name',(#5177),#9365);
#5126=REPRESENTATION('density',(#5027),#9365);
#5127=REPRESENTATION('material name',(#5178),#9366);
#5128=REPRESENTATION('density',(#5028),#9366);
#5129=REPRESENTATION('material name',(#5179),#9367);
#5130=REPRESENTATION('density',(#5029),#9367);
#5131=REPRESENTATION('material name',(#5180),#9368);
#5132=REPRESENTATION('density',(#5030),#9368);
#5133=REPRESENTATION('material name',(#5181),#9369);
#5134=REPRESENTATION('density',(#5031),#9369);
#5135=REPRESENTATION('material name',(#5182),#9370);
#5136=REPRESENTATION('density',(#5032),#9370);
#5137=REPRESENTATION('material name',(#5183),#9371);
#5138=REPRESENTATION('density',(#5033),#9371);
#5139=REPRESENTATION('material name',(#5184),#9372);
#5140=REPRESENTATION('density',(#5034),#9372);
#5141=REPRESENTATION('material name',(#5185),#9374);
#5142=REPRESENTATION('density',(#5035),#9374);
#5143=REPRESENTATION('material name',(#5186),#9375);
#5144=REPRESENTATION('density',(#5036),#9375);
#5145=REPRESENTATION('material name',(#5187),#9376);
#5146=REPRESENTATION('density',(#5037),#9376);
#5147=REPRESENTATION('material name',(#5188),#9377);
#5148=REPRESENTATION('density',(#5038),#9377);
#5149=REPRESENTATION('material name',(#5189),#9379);
#5150=REPRESENTATION('density',(#5039),#9379);
#5151=REPRESENTATION('material name',(#5190),#9380);
#5152=REPRESENTATION('density',(#5040),#9380);
#5153=REPRESENTATION('material name',(#5191),#9381);
#5154=REPRESENTATION('density',(#5041),#9381);
#5155=REPRESENTATION('material name',(#5192),#9382);
#5156=REPRESENTATION('density',(#5042),#9382);
#5157=REPRESENTATION('material name',(#5193),#9383);
#5158=REPRESENTATION('density',(#5043),#9383);
#5159=REPRESENTATION('material name',(#5194),#9384);
#5160=REPRESENTATION('density',(#5044),#9384);
#5161=REPRESENTATION('material name',(#5195),#9386);
#5162=REPRESENTATION('density',(#5045),#9386);
#5163=REPRESENTATION('material name',(#5196),#9387);
#5164=REPRESENTATION('density',(#5046),#9387);
#5165=REPRESENTATION('material name',(#5197),#9388);
#5166=REPRESENTATION('density',(#5047),#9388);
#5167=REPRESENTATION('material name',(#5198),#9390);
#5168=REPRESENTATION('density',(#5048),#9390);
#5169=DESCRIPTIVE_REPRESENTATION_ITEM('Steel','Steel');
#5170=DESCRIPTIVE_REPRESENTATION_ITEM('Steel','Steel');
#5171=DESCRIPTIVE_REPRESENTATION_ITEM('Steel','Steel');
#5172=DESCRIPTIVE_REPRESENTATION_ITEM('Steel','Steel');
#5173=DESCRIPTIVE_REPRESENTATION_ITEM('Steel','Steel');
#5174=DESCRIPTIVE_REPRESENTATION_ITEM('Steel','Steel');
#5175=DESCRIPTIVE_REPRESENTATION_ITEM('Steel','Steel');
#5176=DESCRIPTIVE_REPRESENTATION_ITEM('Steel','Steel');
#5177=DESCRIPTIVE_REPRESENTATION_ITEM('Steel','Steel');
#5178=DESCRIPTIVE_REPRESENTATION_ITEM('Steel','Steel');
#5179=DESCRIPTIVE_REPRESENTATION_ITEM('Steel','Steel');
#5180=DESCRIPTIVE_REPRESENTATION_ITEM('Steel','Steel');
#5181=DESCRIPTIVE_REPRESENTATION_ITEM('Steel','Steel');
#5182=DESCRIPTIVE_REPRESENTATION_ITEM('Steel','Steel');
#5183=DESCRIPTIVE_REPRESENTATION_ITEM('Steel','Steel');
#5184=DESCRIPTIVE_REPRESENTATION_ITEM('Steel','Steel');
#5185=DESCRIPTIVE_REPRESENTATION_ITEM('Steel','Steel');
#5186=DESCRIPTIVE_REPRESENTATION_ITEM('Steel','Steel');
#5187=DESCRIPTIVE_REPRESENTATION_ITEM('Steel','Steel');
#5188=DESCRIPTIVE_REPRESENTATION_ITEM('Steel','Steel');
#5189=DESCRIPTIVE_REPRESENTATION_ITEM('Steel','Steel');
#5190=DESCRIPTIVE_REPRESENTATION_ITEM('Steel','Steel');
#5191=DESCRIPTIVE_REPRESENTATION_ITEM('Steel','Steel');
#5192=DESCRIPTIVE_REPRESENTATION_ITEM('Steel','Steel');
#5193=DESCRIPTIVE_REPRESENTATION_ITEM('Steel','Steel');
#5194=DESCRIPTIVE_REPRESENTATION_ITEM('Steel','Steel');
#5195=DESCRIPTIVE_REPRESENTATION_ITEM('Steel','Steel');
#5196=DESCRIPTIVE_REPRESENTATION_ITEM('Steel','Steel');
#5197=DESCRIPTIVE_REPRESENTATION_ITEM('Steel','Steel');
#5198=DESCRIPTIVE_REPRESENTATION_ITEM('Steel','Steel');
#5199=PROPERTY_DEFINITION('material property','material name',#9559);
#5200=PROPERTY_DEFINITION('material property','density of part',#9559);
#5201=PROPERTY_DEFINITION('material property','material name',#9560);
#5202=PROPERTY_DEFINITION('material property','density of part',#9560);
#5203=PROPERTY_DEFINITION('material property','material name',#9561);
#5204=PROPERTY_DEFINITION('material property','density of part',#9561);
#5205=PROPERTY_DEFINITION('material property','material name',#9562);
#5206=PROPERTY_DEFINITION('material property','density of part',#9562);
#5207=PROPERTY_DEFINITION('material property','material name',#9563);
#5208=PROPERTY_DEFINITION('material property','density of part',#9563);
#5209=PROPERTY_DEFINITION('material property','material name',#9564);
#5210=PROPERTY_DEFINITION('material property','density of part',#9564);
#5211=PROPERTY_DEFINITION('material property','material name',#9565);
#5212=PROPERTY_DEFINITION('material property','density of part',#9565);
#5213=PROPERTY_DEFINITION('material property','material name',#9566);
#5214=PROPERTY_DEFINITION('material property','density of part',#9566);
#5215=PROPERTY_DEFINITION('material property','material name',#9567);
#5216=PROPERTY_DEFINITION('material property','density of part',#9567);
#5217=PROPERTY_DEFINITION('material property','material name',#9568);
#5218=PROPERTY_DEFINITION('material property','density of part',#9568);
#5219=PROPERTY_DEFINITION('material property','material name',#9569);
#5220=PROPERTY_DEFINITION('material property','density of part',#9569);
#5221=PROPERTY_DEFINITION('material property','material name',#9570);
#5222=PROPERTY_DEFINITION('material property','density of part',#9570);
#5223=PROPERTY_DEFINITION('material property','material name',#9571);
#5224=PROPERTY_DEFINITION('material property','density of part',#9571);
#5225=PROPERTY_DEFINITION('material property','material name',#9572);
#5226=PROPERTY_DEFINITION('material property','density of part',#9572);
#5227=PROPERTY_DEFINITION('material property','material name',#9573);
#5228=PROPERTY_DEFINITION('material property','density of part',#9573);
#5229=PROPERTY_DEFINITION('material property','material name',#9574);
#5230=PROPERTY_DEFINITION('material property','density of part',#9574);
#5231=PROPERTY_DEFINITION('material property','material name',#9576);
#5232=PROPERTY_DEFINITION('material property','density of part',#9576);
#5233=PROPERTY_DEFINITION('material property','material name',#9577);
#5234=PROPERTY_DEFINITION('material property','density of part',#9577);
#5235=PROPERTY_DEFINITION('material property','material name',#9578);
#5236=PROPERTY_DEFINITION('material property','density of part',#9578);
#5237=PROPERTY_DEFINITION('material property','material name',#9579);
#5238=PROPERTY_DEFINITION('material property','density of part',#9579);
#5239=PROPERTY_DEFINITION('material property','material name',#9581);
#5240=PROPERTY_DEFINITION('material property','density of part',#9581);
#5241=PROPERTY_DEFINITION('material property','material name',#9582);
#5242=PROPERTY_DEFINITION('material property','density of part',#9582);
#5243=PROPERTY_DEFINITION('material property','material name',#9583);
#5244=PROPERTY_DEFINITION('material property','density of part',#9583);
#5245=PROPERTY_DEFINITION('material property','material name',#9584);
#5246=PROPERTY_DEFINITION('material property','density of part',#9584);
#5247=PROPERTY_DEFINITION('material property','material name',#9585);
#5248=PROPERTY_DEFINITION('material property','density of part',#9585);
#5249=PROPERTY_DEFINITION('material property','material name',#9586);
#5250=PROPERTY_DEFINITION('material property','density of part',#9586);
#5251=PROPERTY_DEFINITION('material property','material name',#9588);
#5252=PROPERTY_DEFINITION('material property','density of part',#9588);
#5253=PROPERTY_DEFINITION('material property','material name',#9589);
#5254=PROPERTY_DEFINITION('material property','density of part',#9589);
#5255=PROPERTY_DEFINITION('material property','material name',#9590);
#5256=PROPERTY_DEFINITION('material property','density of part',#9590);
#5257=PROPERTY_DEFINITION('material property','material name',#9592);
#5258=PROPERTY_DEFINITION('material property','density of part',#9592);
#5259=AXIS2_PLACEMENT_3D('',#7557,#5929,#5930);
#5260=AXIS2_PLACEMENT_3D('',#7558,#5931,#5932);
#5261=AXIS2_PLACEMENT_3D('',#7559,#5933,#5934);
#5262=AXIS2_PLACEMENT_3D('',#7560,#5935,#5936);
#5263=AXIS2_PLACEMENT_3D('',#7563,#5937,#5938);
#5264=AXIS2_PLACEMENT_3D('',#7565,#5939,#5940);
#5265=AXIS2_PLACEMENT_3D('',#7567,#5941,#5942);
#5266=AXIS2_PLACEMENT_3D('',#7569,#5943,#5944);
#5267=AXIS2_PLACEMENT_3D('',#7571,#5945,#5946);
#5268=AXIS2_PLACEMENT_3D('',#7573,#5947,#5948);
#5269=AXIS2_PLACEMENT_3D('',#7575,#5949,#5950);
#5270=AXIS2_PLACEMENT_3D('',#7576,#5951,#5952);
#5271=AXIS2_PLACEMENT_3D('',#7578,#5953,#5954);
#5272=AXIS2_PLACEMENT_3D('',#7579,#5955,#5956);
#5273=AXIS2_PLACEMENT_3D('',#7584,#5959,#5960);
#5274=AXIS2_PLACEMENT_3D('',#7585,#5961,#5962);
#5275=AXIS2_PLACEMENT_3D('',#7589,#5964,#5965);
#5276=AXIS2_PLACEMENT_3D('',#7591,#5967,#5968);
#5277=AXIS2_PLACEMENT_3D('',#7596,#5971,#5972);
#5278=AXIS2_PLACEMENT_3D('',#7597,#5973,#5974);
#5279=AXIS2_PLACEMENT_3D('',#7600,#5976,#5977);
#5280=AXIS2_PLACEMENT_3D('',#7601,#5978,#5979);
#5281=AXIS2_PLACEMENT_3D('',#7605,#5981,#5982);
#5282=AXIS2_PLACEMENT_3D('',#7607,#5984,#5985);
#5283=AXIS2_PLACEMENT_3D('',#7609,#5986,#5987);
#5284=AXIS2_PLACEMENT_3D('',#7612,#5989,#5990);
#5285=AXIS2_PLACEMENT_3D('',#7613,#5991,#5992);
#5286=AXIS2_PLACEMENT_3D('',#7614,#5993,#5994);
#5287=AXIS2_PLACEMENT_3D('',#7616,#5995,#5996);
#5288=AXIS2_PLACEMENT_3D('',#7619,#5998,#5999);
#5289=AXIS2_PLACEMENT_3D('',#7620,#6000,#6001);
#5290=AXIS2_PLACEMENT_3D('',#7621,#6002,#6003);
#5291=AXIS2_PLACEMENT_3D('',#7623,#6004,#6005);
#5292=AXIS2_PLACEMENT_3D('',#7626,#6007,#6008);
#5293=AXIS2_PLACEMENT_3D('',#7627,#6009,#6010);
#5294=AXIS2_PLACEMENT_3D('',#7628,#6011,#6012);
#5295=AXIS2_PLACEMENT_3D('',#7630,#6013,#6014);
#5296=AXIS2_PLACEMENT_3D('',#7631,#6015,#6016);
#5297=AXIS2_PLACEMENT_3D('',#7633,#6017,#6018);
#5298=AXIS2_PLACEMENT_3D('',#7636,#6020,#6021);
#5299=AXIS2_PLACEMENT_3D('',#7637,#6022,#6023);
#5300=AXIS2_PLACEMENT_3D('',#7638,#6024,#6025);
#5301=AXIS2_PLACEMENT_3D('',#7640,#6026,#6027);
#5302=AXIS2_PLACEMENT_3D('',#7643,#6029,#6030);
#5303=AXIS2_PLACEMENT_3D('',#7644,#6031,#6032);
#5304=AXIS2_PLACEMENT_3D('',#7646,#6033,#6034);
#5305=AXIS2_PLACEMENT_3D('',#7649,#6036,#6037);
#5306=AXIS2_PLACEMENT_3D('',#7650,#6038,#6039);
#5307=AXIS2_PLACEMENT_3D('',#7652,#6040,#6041);
#5308=AXIS2_PLACEMENT_3D('',#7655,#6043,#6044);
#5309=AXIS2_PLACEMENT_3D('',#7656,#6045,#6046);
#5310=AXIS2_PLACEMENT_3D('',#7658,#6047,#6048);
#5311=AXIS2_PLACEMENT_3D('',#7660,#6050,#6051);
#5312=AXIS2_PLACEMENT_3D('',#7669,#6056,#6057);
#5313=AXIS2_PLACEMENT_3D('',#7675,#6061,#6062);
#5314=AXIS2_PLACEMENT_3D('',#7681,#6066,#6067);
#5315=AXIS2_PLACEMENT_3D('',#7687,#6071,#6072);
#5316=AXIS2_PLACEMENT_3D('',#7693,#6076,#6077);
#5317=AXIS2_PLACEMENT_3D('',#7699,#6081,#6082);
#5318=AXIS2_PLACEMENT_3D('',#7705,#6086,#6087);
#5319=AXIS2_PLACEMENT_3D('',#7708,#6090,#6091);
#5320=AXIS2_PLACEMENT_3D('',#7709,#6092,#6093);
#5321=AXIS2_PLACEMENT_3D('',#7710,#6094,#6095);
#5322=AXIS2_PLACEMENT_3D('',#7711,#6096,#6097);
#5323=AXIS2_PLACEMENT_3D('',#7714,#6098,#6099);
#5324=AXIS2_PLACEMENT_3D('',#7716,#6100,#6101);
#5325=AXIS2_PLACEMENT_3D('',#7718,#6102,#6103);
#5326=AXIS2_PLACEMENT_3D('',#7720,#6104,#6105);
#5327=AXIS2_PLACEMENT_3D('',#7722,#6106,#6107);
#5328=AXIS2_PLACEMENT_3D('',#7724,#6108,#6109);
#5329=AXIS2_PLACEMENT_3D('',#7726,#6110,#6111);
#5330=AXIS2_PLACEMENT_3D('',#7727,#6112,#6113);
#5331=AXIS2_PLACEMENT_3D('',#7729,#6114,#6115);
#5332=AXIS2_PLACEMENT_3D('',#7730,#6116,#6117);
#5333=AXIS2_PLACEMENT_3D('',#7735,#6120,#6121);
#5334=AXIS2_PLACEMENT_3D('',#7736,#6122,#6123);
#5335=AXIS2_PLACEMENT_3D('',#7741,#6126,#6127);
#5336=AXIS2_PLACEMENT_3D('',#7742,#6128,#6129);
#5337=AXIS2_PLACEMENT_3D('',#7746,#6131,#6132);
#5338=AXIS2_PLACEMENT_3D('',#7748,#6134,#6135);
#5339=AXIS2_PLACEMENT_3D('',#7750,#6136,#6137);
#5340=AXIS2_PLACEMENT_3D('',#7752,#6139,#6140);
#5341=AXIS2_PLACEMENT_3D('',#7756,#6142,#6143);
#5342=AXIS2_PLACEMENT_3D('',#7758,#6145,#6146);
#5343=AXIS2_PLACEMENT_3D('',#7760,#6147,#6148);
#5344=AXIS2_PLACEMENT_3D('',#7763,#6150,#6151);
#5345=AXIS2_PLACEMENT_3D('',#7764,#6152,#6153);
#5346=AXIS2_PLACEMENT_3D('',#7765,#6154,#6155);
#5347=AXIS2_PLACEMENT_3D('',#7767,#6156,#6157);
#5348=AXIS2_PLACEMENT_3D('',#7770,#6159,#6160);
#5349=AXIS2_PLACEMENT_3D('',#7771,#6161,#6162);
#5350=AXIS2_PLACEMENT_3D('',#7772,#6163,#6164);
#5351=AXIS2_PLACEMENT_3D('',#7774,#6165,#6166);
#5352=AXIS2_PLACEMENT_3D('',#7775,#6167,#6168);
#5353=AXIS2_PLACEMENT_3D('',#7777,#6169,#6170);
#5354=AXIS2_PLACEMENT_3D('',#7780,#6172,#6173);
#5355=AXIS2_PLACEMENT_3D('',#7781,#6174,#6175);
#5356=AXIS2_PLACEMENT_3D('',#7782,#6176,#6177);
#5357=AXIS2_PLACEMENT_3D('',#7784,#6178,#6179);
#5358=AXIS2_PLACEMENT_3D('',#7787,#6181,#6182);
#5359=AXIS2_PLACEMENT_3D('',#7788,#6183,#6184);
#5360=AXIS2_PLACEMENT_3D('',#7789,#6185,#6186);
#5361=AXIS2_PLACEMENT_3D('',#7791,#6187,#6188);
#5362=AXIS2_PLACEMENT_3D('',#7794,#6190,#6191);
#5363=AXIS2_PLACEMENT_3D('',#7795,#6192,#6193);
#5364=AXIS2_PLACEMENT_3D('',#7797,#6194,#6195);
#5365=AXIS2_PLACEMENT_3D('',#7800,#6197,#6198);
#5366=AXIS2_PLACEMENT_3D('',#7801,#6199,#6200);
#5367=AXIS2_PLACEMENT_3D('',#7803,#6201,#6202);
#5368=AXIS2_PLACEMENT_3D('',#7806,#6204,#6205);
#5369=AXIS2_PLACEMENT_3D('',#7807,#6206,#6207);
#5370=AXIS2_PLACEMENT_3D('',#7810,#6209,#6210);
#5371=AXIS2_PLACEMENT_3D('',#7811,#6211,#6212);
#5372=AXIS2_PLACEMENT_3D('',#7820,#6217,#6218);
#5373=AXIS2_PLACEMENT_3D('',#7826,#6222,#6223);
#5374=AXIS2_PLACEMENT_3D('',#7832,#6227,#6228);
#5375=AXIS2_PLACEMENT_3D('',#7838,#6232,#6233);
#5376=AXIS2_PLACEMENT_3D('',#7844,#6237,#6238);
#5377=AXIS2_PLACEMENT_3D('',#7850,#6242,#6243);
#5378=AXIS2_PLACEMENT_3D('',#7856,#6247,#6248);
#5379=AXIS2_PLACEMENT_3D('',#7859,#6251,#6252);
#5380=AXIS2_PLACEMENT_3D('',#7860,#6253,#6254);
#5381=AXIS2_PLACEMENT_3D('',#7861,#6255,#6256);
#5382=AXIS2_PLACEMENT_3D('',#7862,#6257,#6258);
#5383=AXIS2_PLACEMENT_3D('',#7864,#6259,#6260);
#5384=AXIS2_PLACEMENT_3D('',#7867,#6262,#6263);
#5385=AXIS2_PLACEMENT_3D('',#7868,#6264,#6265);
#5386=AXIS2_PLACEMENT_3D('',#7870,#6266,#6267);
#5387=AXIS2_PLACEMENT_3D('',#7873,#6269,#6270);
#5388=AXIS2_PLACEMENT_3D('',#7874,#6271,#6272);
#5389=AXIS2_PLACEMENT_3D('',#7876,#6273,#6274);
#5390=AXIS2_PLACEMENT_3D('',#7879,#6276,#6277);
#5391=AXIS2_PLACEMENT_3D('',#7880,#6278,#6279);
#5392=AXIS2_PLACEMENT_3D('',#7889,#6284,#6285);
#5393=AXIS2_PLACEMENT_3D('',#7895,#6289,#6290);
#5394=AXIS2_PLACEMENT_3D('',#7901,#6294,#6295);
#5395=AXIS2_PLACEMENT_3D('',#7904,#6298,#6299);
#5396=AXIS2_PLACEMENT_3D('',#7905,#6300,#6301);
#5397=AXIS2_PLACEMENT_3D('',#7906,#6302,#6303);
#5398=AXIS2_PLACEMENT_3D('',#7907,#6304,#6305);
#5399=AXIS2_PLACEMENT_3D('',#7909,#6306,#6307);
#5400=AXIS2_PLACEMENT_3D('',#7912,#6309,#6310);
#5401=AXIS2_PLACEMENT_3D('',#7913,#6311,#6312);
#5402=AXIS2_PLACEMENT_3D('',#7915,#6313,#6314);
#5403=AXIS2_PLACEMENT_3D('',#7918,#6316,#6317);
#5404=AXIS2_PLACEMENT_3D('',#7919,#6318,#6319);
#5405=AXIS2_PLACEMENT_3D('',#7920,#6320,#6321);
#5406=AXIS2_PLACEMENT_3D('',#7921,#6322,#6323);
#5407=AXIS2_PLACEMENT_3D('',#7922,#6324,#6325);
#5408=AXIS2_PLACEMENT_3D('',#7924,#6326,#6327);
#5409=AXIS2_PLACEMENT_3D('',#7927,#6329,#6330);
#5410=AXIS2_PLACEMENT_3D('',#7928,#6331,#6332);
#5411=AXIS2_PLACEMENT_3D('',#7929,#6333,#6334);
#5412=AXIS2_PLACEMENT_3D('',#7931,#6335,#6336);
#5413=AXIS2_PLACEMENT_3D('',#7933,#6337,#6338);
#5414=AXIS2_PLACEMENT_3D('',#7934,#6339,#6340);
#5415=AXIS2_PLACEMENT_3D('',#7937,#6342,#6343);
#5416=AXIS2_PLACEMENT_3D('',#7938,#6344,#6345);
#5417=AXIS2_PLACEMENT_3D('',#7939,#6346,#6347);
#5418=AXIS2_PLACEMENT_3D('',#7941,#6348,#6349);
#5419=AXIS2_PLACEMENT_3D('',#7943,#6351,#6352);
#5420=AXIS2_PLACEMENT_3D('',#7944,#6353,#6354);
#5421=AXIS2_PLACEMENT_3D('',#7945,#6355,#6356);
#5422=AXIS2_PLACEMENT_3D('',#7947,#6357,#6358);
#5423=AXIS2_PLACEMENT_3D('',#7950,#6360,#6361);
#5424=AXIS2_PLACEMENT_3D('',#7951,#6362,#6363);
#5425=AXIS2_PLACEMENT_3D('',#7953,#6364,#6365);
#5426=AXIS2_PLACEMENT_3D('',#7956,#6367,#6368);
#5427=AXIS2_PLACEMENT_3D('',#7957,#6369,#6370);
#5428=AXIS2_PLACEMENT_3D('',#7958,#6371,#6372);
#5429=AXIS2_PLACEMENT_3D('',#7959,#6373,#6374);
#5430=AXIS2_PLACEMENT_3D('',#7960,#6375,#6376);
#5431=AXIS2_PLACEMENT_3D('',#7962,#6377,#6378);
#5432=AXIS2_PLACEMENT_3D('',#7965,#6380,#6381);
#5433=AXIS2_PLACEMENT_3D('',#7966,#6382,#6383);
#5434=AXIS2_PLACEMENT_3D('',#7968,#6384,#6385);
#5435=AXIS2_PLACEMENT_3D('',#7971,#6387,#6388);
#5436=AXIS2_PLACEMENT_3D('',#7972,#6389,#6390);
#5437=AXIS2_PLACEMENT_3D('',#7973,#6391,#6392);
#5438=AXIS2_PLACEMENT_3D('',#7974,#6393,#6394);
#5439=AXIS2_PLACEMENT_3D('',#7975,#6395,#6396);
#5440=AXIS2_PLACEMENT_3D('',#7977,#6397,#6398);
#5441=AXIS2_PLACEMENT_3D('',#7980,#6400,#6401);
#5442=AXIS2_PLACEMENT_3D('',#7981,#6402,#6403);
#5443=AXIS2_PLACEMENT_3D('',#7983,#6404,#6405);
#5444=AXIS2_PLACEMENT_3D('',#7986,#6407,#6408);
#5445=AXIS2_PLACEMENT_3D('',#7987,#6409,#6410);
#5446=AXIS2_PLACEMENT_3D('',#7988,#6411,#6412);
#5447=AXIS2_PLACEMENT_3D('',#7989,#6413,#6414);
#5448=AXIS2_PLACEMENT_3D('',#7990,#6415,#6416);
#5449=AXIS2_PLACEMENT_3D('',#7992,#6417,#6418);
#5450=AXIS2_PLACEMENT_3D('',#7995,#6420,#6421);
#5451=AXIS2_PLACEMENT_3D('',#7996,#6422,#6423);
#5452=AXIS2_PLACEMENT_3D('',#7998,#6424,#6425);
#5453=AXIS2_PLACEMENT_3D('',#8001,#6427,#6428);
#5454=AXIS2_PLACEMENT_3D('',#8002,#6429,#6430);
#5455=AXIS2_PLACEMENT_3D('',#8003,#6431,#6432);
#5456=AXIS2_PLACEMENT_3D('',#8004,#6433,#6434);
#5457=AXIS2_PLACEMENT_3D('',#8005,#6435,#6436);
#5458=AXIS2_PLACEMENT_3D('',#8007,#6437,#6438);
#5459=AXIS2_PLACEMENT_3D('',#8010,#6440,#6441);
#5460=AXIS2_PLACEMENT_3D('',#8011,#6442,#6443);
#5461=AXIS2_PLACEMENT_3D('',#8013,#6444,#6445);
#5462=AXIS2_PLACEMENT_3D('',#8016,#6447,#6448);
#5463=AXIS2_PLACEMENT_3D('',#8017,#6449,#6450);
#5464=AXIS2_PLACEMENT_3D('',#8018,#6451,#6452);
#5465=AXIS2_PLACEMENT_3D('',#8019,#6453,#6454);
#5466=AXIS2_PLACEMENT_3D('',#8020,#6455,#6456);
#5467=AXIS2_PLACEMENT_3D('',#8022,#6457,#6458);
#5468=AXIS2_PLACEMENT_3D('',#8025,#6460,#6461);
#5469=AXIS2_PLACEMENT_3D('',#8026,#6462,#6463);
#5470=AXIS2_PLACEMENT_3D('',#8028,#6464,#6465);
#5471=AXIS2_PLACEMENT_3D('',#8031,#6467,#6468);
#5472=AXIS2_PLACEMENT_3D('',#8032,#6469,#6470);
#5473=AXIS2_PLACEMENT_3D('',#8033,#6471,#6472);
#5474=AXIS2_PLACEMENT_3D('',#8034,#6473,#6474);
#5475=AXIS2_PLACEMENT_3D('',#8035,#6475,#6476);
#5476=AXIS2_PLACEMENT_3D('',#8037,#6477,#6478);
#5477=AXIS2_PLACEMENT_3D('',#8040,#6480,#6481);
#5478=AXIS2_PLACEMENT_3D('',#8041,#6482,#6483);
#5479=AXIS2_PLACEMENT_3D('',#8043,#6484,#6485);
#5480=AXIS2_PLACEMENT_3D('',#8046,#6487,#6488);
#5481=AXIS2_PLACEMENT_3D('',#8047,#6489,#6490);
#5482=AXIS2_PLACEMENT_3D('',#8048,#6491,#6492);
#5483=AXIS2_PLACEMENT_3D('',#8049,#6493,#6494);
#5484=AXIS2_PLACEMENT_3D('',#8050,#6495,#6496);
#5485=AXIS2_PLACEMENT_3D('',#8059,#6501,#6502);
#5486=AXIS2_PLACEMENT_3D('',#8065,#6506,#6507);
#5487=AXIS2_PLACEMENT_3D('',#8071,#6511,#6512);
#5488=AXIS2_PLACEMENT_3D('',#8077,#6516,#6517);
#5489=AXIS2_PLACEMENT_3D('',#8083,#6521,#6522);
#5490=AXIS2_PLACEMENT_3D('',#8086,#6525,#6526);
#5491=AXIS2_PLACEMENT_3D('',#8087,#6527,#6528);
#5492=AXIS2_PLACEMENT_3D('',#8088,#6529,#6530);
#5493=AXIS2_PLACEMENT_3D('',#8090,#6531,#6532);
#5494=AXIS2_PLACEMENT_3D('',#8092,#6533,#6534);
#5495=AXIS2_PLACEMENT_3D('',#8093,#6535,#6536);
#5496=AXIS2_PLACEMENT_3D('',#8096,#6538,#6539);
#5497=AXIS2_PLACEMENT_3D('',#8097,#6540,#6541);
#5498=AXIS2_PLACEMENT_3D('',#8098,#6542,#6543);
#5499=AXIS2_PLACEMENT_3D('',#8100,#6544,#6545);
#5500=AXIS2_PLACEMENT_3D('',#8101,#6546,#6547);
#5501=AXIS2_PLACEMENT_3D('',#8103,#6548,#6549);
#5502=AXIS2_PLACEMENT_3D('',#8105,#6551,#6552);
#5503=AXIS2_PLACEMENT_3D('',#8107,#6553,#6554);
#5504=AXIS2_PLACEMENT_3D('',#8109,#6556,#6557);
#5505=AXIS2_PLACEMENT_3D('',#8111,#6558,#6559);
#5506=AXIS2_PLACEMENT_3D('',#8113,#6561,#6562);
#5507=AXIS2_PLACEMENT_3D('',#8115,#6563,#6564);
#5508=AXIS2_PLACEMENT_3D('',#8116,#6565,#6566);
#5509=AXIS2_PLACEMENT_3D('',#8118,#6567,#6568);
#5510=AXIS2_PLACEMENT_3D('',#8120,#6570,#6571);
#5511=AXIS2_PLACEMENT_3D('',#8122,#6573,#6574);
#5512=AXIS2_PLACEMENT_3D('',#8123,#6575,#6576);
#5513=AXIS2_PLACEMENT_3D('',#8125,#6577,#6578);
#5514=AXIS2_PLACEMENT_3D('',#8128,#6580,#6581);
#5515=AXIS2_PLACEMENT_3D('',#8129,#6582,#6583);
#5516=AXIS2_PLACEMENT_3D('',#8131,#6584,#6585);
#5517=AXIS2_PLACEMENT_3D('',#8134,#6587,#6588);
#5518=AXIS2_PLACEMENT_3D('',#8135,#6589,#6590);
#5519=AXIS2_PLACEMENT_3D('',#8136,#6591,#6592);
#5520=AXIS2_PLACEMENT_3D('',#8137,#6593,#6594);
#5521=AXIS2_PLACEMENT_3D('',#8138,#6595,#6596);
#5522=AXIS2_PLACEMENT_3D('',#8150,#6598,#6599);
#5523=AXIS2_PLACEMENT_3D('',#8166,#6600,#6601);
#5524=AXIS2_PLACEMENT_3D('',#8168,#6602,#6603);
#5525=AXIS2_PLACEMENT_3D('',#8194,#6605,#6606);
#5526=AXIS2_PLACEMENT_3D('',#8197,#6609,#6610);
#5527=AXIS2_PLACEMENT_3D('',#8199,#6612,#6613);
#5528=AXIS2_PLACEMENT_3D('',#8201,#6615,#6616);
#5529=AXIS2_PLACEMENT_3D('',#8203,#6617,#6618);
#5530=AXIS2_PLACEMENT_3D('',#8206,#6620,#6621);
#5531=AXIS2_PLACEMENT_3D('',#8207,#6622,#6623);
#5532=AXIS2_PLACEMENT_3D('',#8209,#6625,#6626);
#5533=AXIS2_PLACEMENT_3D('',#8211,#6628,#6629);
#5534=AXIS2_PLACEMENT_3D('',#8212,#6630,#6631);
#5535=AXIS2_PLACEMENT_3D('',#8213,#6632,#6633);
#5536=AXIS2_PLACEMENT_3D('',#8214,#6634,#6635);
#5537=AXIS2_PLACEMENT_3D('',#8215,#6636,#6637);
#5538=AXIS2_PLACEMENT_3D('',#8217,#6638,#6639);
#5539=AXIS2_PLACEMENT_3D('',#8218,#6640,#6641);
#5540=AXIS2_PLACEMENT_3D('',#8220,#6642,#6643);
#5541=AXIS2_PLACEMENT_3D('',#8222,#6645,#6646);
#5542=AXIS2_PLACEMENT_3D('',#8224,#6647,#6648);
#5543=AXIS2_PLACEMENT_3D('',#8226,#6650,#6651);
#5544=AXIS2_PLACEMENT_3D('',#8228,#6652,#6653);
#5545=AXIS2_PLACEMENT_3D('',#8230,#6655,#6656);
#5546=AXIS2_PLACEMENT_3D('',#8232,#6657,#6658);
#5547=AXIS2_PLACEMENT_3D('',#8233,#6659,#6660);
#5548=AXIS2_PLACEMENT_3D('',#8235,#6661,#6662);
#5549=AXIS2_PLACEMENT_3D('',#8237,#6664,#6665);
#5550=AXIS2_PLACEMENT_3D('',#8239,#6666,#6667);
#5551=AXIS2_PLACEMENT_3D('',#8241,#6669,#6670);
#5552=AXIS2_PLACEMENT_3D('',#8243,#6671,#6672);
#5553=AXIS2_PLACEMENT_3D('',#8245,#6674,#6675);
#5554=AXIS2_PLACEMENT_3D('',#8246,#6676,#6677);
#5555=AXIS2_PLACEMENT_3D('',#8255,#6682,#6683);
#5556=AXIS2_PLACEMENT_3D('',#8261,#6687,#6688);
#5557=AXIS2_PLACEMENT_3D('',#8267,#6692,#6693);
#5558=AXIS2_PLACEMENT_3D('',#8273,#6697,#6698);
#5559=AXIS2_PLACEMENT_3D('',#8279,#6702,#6703);
#5560=AXIS2_PLACEMENT_3D('',#8282,#6706,#6707);
#5561=AXIS2_PLACEMENT_3D('',#8283,#6708,#6709);
#5562=AXIS2_PLACEMENT_3D('',#8284,#6710,#6711);
#5563=AXIS2_PLACEMENT_3D('',#8285,#6712,#6713);
#5564=AXIS2_PLACEMENT_3D('',#8286,#6714,#6715);
#5565=AXIS2_PLACEMENT_3D('',#8287,#6716,#6717);
#5566=AXIS2_PLACEMENT_3D('',#8288,#6718,#6719);
#5567=AXIS2_PLACEMENT_3D('',#8289,#6720,#6721);
#5568=AXIS2_PLACEMENT_3D('',#8290,#6722,#6723);
#5569=AXIS2_PLACEMENT_3D('',#8291,#6724,#6725);
#5570=AXIS2_PLACEMENT_3D('',#8292,#6726,#6727);
#5571=AXIS2_PLACEMENT_3D('',#8293,#6728,#6729);
#5572=AXIS2_PLACEMENT_3D('',#8294,#6730,#6731);
#5573=AXIS2_PLACEMENT_3D('',#8295,#6732,#6733);
#5574=AXIS2_PLACEMENT_3D('',#8296,#6734,#6735);
#5575=AXIS2_PLACEMENT_3D('',#8297,#6736,#6737);
#5576=AXIS2_PLACEMENT_3D('',#8298,#6738,#6739);
#5577=AXIS2_PLACEMENT_3D('',#8299,#6740,#6741);
#5578=AXIS2_PLACEMENT_3D('',#8300,#6742,#6743);
#5579=AXIS2_PLACEMENT_3D('',#8301,#6744,#6745);
#5580=AXIS2_PLACEMENT_3D('',#8302,#6746,#6747);
#5581=AXIS2_PLACEMENT_3D('',#8303,#6748,#6749);
#5582=AXIS2_PLACEMENT_3D('',#8304,#6750,#6751);
#5583=AXIS2_PLACEMENT_3D('',#8305,#6752,#6753);
#5584=AXIS2_PLACEMENT_3D('',#8306,#6754,#6755);
#5585=AXIS2_PLACEMENT_3D('',#8307,#6756,#6757);
#5586=AXIS2_PLACEMENT_3D('',#8308,#6758,#6759);
#5587=AXIS2_PLACEMENT_3D('',#8309,#6760,#6761);
#5588=AXIS2_PLACEMENT_3D('',#8310,#6762,#6763);
#5589=AXIS2_PLACEMENT_3D('',#8311,#6764,#6765);
#5590=AXIS2_PLACEMENT_3D('',#8313,#6766,#6767);
#5591=AXIS2_PLACEMENT_3D('',#8316,#6769,#6770);
#5592=AXIS2_PLACEMENT_3D('',#8317,#6771,#6772);
#5593=AXIS2_PLACEMENT_3D('',#8319,#6773,#6774);
#5594=AXIS2_PLACEMENT_3D('',#8322,#6776,#6777);
#5595=AXIS2_PLACEMENT_3D('',#8323,#6778,#6779);
#5596=AXIS2_PLACEMENT_3D('',#8325,#6780,#6781);
#5597=AXIS2_PLACEMENT_3D('',#8328,#6783,#6784);
#5598=AXIS2_PLACEMENT_3D('',#8329,#6785,#6786);
#5599=AXIS2_PLACEMENT_3D('',#8331,#6787,#6788);
#5600=AXIS2_PLACEMENT_3D('',#8334,#6790,#6791);
#5601=AXIS2_PLACEMENT_3D('',#8335,#6792,#6793);
#5602=AXIS2_PLACEMENT_3D('',#8337,#6794,#6795);
#5603=AXIS2_PLACEMENT_3D('',#8340,#6797,#6798);
#5604=AXIS2_PLACEMENT_3D('',#8341,#6799,#6800);
#5605=AXIS2_PLACEMENT_3D('',#8343,#6801,#6802);
#5606=AXIS2_PLACEMENT_3D('',#8345,#6804,#6805);
#5607=AXIS2_PLACEMENT_3D('',#8347,#6806,#6807);
#5608=AXIS2_PLACEMENT_3D('',#8349,#6809,#6810);
#5609=AXIS2_PLACEMENT_3D('',#8351,#6811,#6812);
#5610=AXIS2_PLACEMENT_3D('',#8352,#6813,#6814);
#5611=AXIS2_PLACEMENT_3D('',#8354,#6815,#6816);
#5612=AXIS2_PLACEMENT_3D('',#8356,#6817,#6818);
#5613=AXIS2_PLACEMENT_3D('',#8357,#6819,#6820);
#5614=AXIS2_PLACEMENT_3D('',#8359,#6822,#6823);
#5615=AXIS2_PLACEMENT_3D('',#8362,#6825,#6826);
#5616=AXIS2_PLACEMENT_3D('',#8363,#6827,#6828);
#5617=AXIS2_PLACEMENT_3D('',#8365,#6829,#6830);
#5618=AXIS2_PLACEMENT_3D('',#8368,#6832,#6833);
#5619=AXIS2_PLACEMENT_3D('',#8369,#6834,#6835);
#5620=AXIS2_PLACEMENT_3D('',#8371,#6836,#6837);
#5621=AXIS2_PLACEMENT_3D('',#8373,#6839,#6840);
#5622=AXIS2_PLACEMENT_3D('',#8374,#6841,#6842);
#5623=AXIS2_PLACEMENT_3D('',#8375,#6843,#6844);
#5624=AXIS2_PLACEMENT_3D('',#8376,#6845,#6846);
#5625=AXIS2_PLACEMENT_3D('',#8378,#6847,#6848);
#5626=AXIS2_PLACEMENT_3D('',#8381,#6850,#6851);
#5627=AXIS2_PLACEMENT_3D('',#8382,#6852,#6853);
#5628=AXIS2_PLACEMENT_3D('',#8384,#6854,#6855);
#5629=AXIS2_PLACEMENT_3D('',#8387,#6857,#6858);
#5630=AXIS2_PLACEMENT_3D('',#8388,#6859,#6860);
#5631=AXIS2_PLACEMENT_3D('',#8389,#6861,#6862);
#5632=AXIS2_PLACEMENT_3D('',#8390,#6863,#6864);
#5633=AXIS2_PLACEMENT_3D('',#8391,#6865,#6866);
#5634=AXIS2_PLACEMENT_3D('',#8393,#6867,#6868);
#5635=AXIS2_PLACEMENT_3D('',#8396,#6870,#6871);
#5636=AXIS2_PLACEMENT_3D('',#8397,#6872,#6873);
#5637=AXIS2_PLACEMENT_3D('',#8399,#6874,#6875);
#5638=AXIS2_PLACEMENT_3D('',#8402,#6877,#6878);
#5639=AXIS2_PLACEMENT_3D('',#8403,#6879,#6880);
#5640=AXIS2_PLACEMENT_3D('',#8405,#6881,#6882);
#5641=AXIS2_PLACEMENT_3D('',#8408,#6884,#6885);
#5642=AXIS2_PLACEMENT_3D('',#8409,#6886,#6887);
#5643=AXIS2_PLACEMENT_3D('',#8411,#6888,#6889);
#5644=AXIS2_PLACEMENT_3D('',#8414,#6891,#6892);
#5645=AXIS2_PLACEMENT_3D('',#8415,#6893,#6894);
#5646=AXIS2_PLACEMENT_3D('',#8417,#6895,#6896);
#5647=AXIS2_PLACEMENT_3D('',#8420,#6898,#6899);
#5648=AXIS2_PLACEMENT_3D('',#8421,#6900,#6901);
#5649=AXIS2_PLACEMENT_3D('',#8423,#6902,#6903);
#5650=AXIS2_PLACEMENT_3D('',#8424,#6904,#6905);
#5651=AXIS2_PLACEMENT_3D('',#8427,#6907,#6908);
#5652=AXIS2_PLACEMENT_3D('',#8428,#6909,#6910);
#5653=AXIS2_PLACEMENT_3D('',#8430,#6911,#6912);
#5654=AXIS2_PLACEMENT_3D('',#8433,#6914,#6915);
#5655=AXIS2_PLACEMENT_3D('',#8434,#6916,#6917);
#5656=AXIS2_PLACEMENT_3D('',#8435,#6918,#6919);
#5657=AXIS2_PLACEMENT_3D('',#8436,#6920,#6921);
#5658=AXIS2_PLACEMENT_3D('',#8437,#6922,#6923);
#5659=AXIS2_PLACEMENT_3D('',#8439,#6924,#6925);
#5660=AXIS2_PLACEMENT_3D('',#8442,#6927,#6928);
#5661=AXIS2_PLACEMENT_3D('',#8443,#6929,#6930);
#5662=AXIS2_PLACEMENT_3D('',#8445,#6931,#6932);
#5663=AXIS2_PLACEMENT_3D('',#8448,#6934,#6935);
#5664=AXIS2_PLACEMENT_3D('',#8449,#6936,#6937);
#5665=AXIS2_PLACEMENT_3D('',#8451,#6938,#6939);
#5666=AXIS2_PLACEMENT_3D('',#8454,#6941,#6942);
#5667=AXIS2_PLACEMENT_3D('',#8455,#6943,#6944);
#5668=AXIS2_PLACEMENT_3D('',#8457,#6945,#6946);
#5669=AXIS2_PLACEMENT_3D('',#8460,#6948,#6949);
#5670=AXIS2_PLACEMENT_3D('',#8461,#6950,#6951);
#5671=AXIS2_PLACEMENT_3D('',#8463,#6952,#6953);
#5672=AXIS2_PLACEMENT_3D('',#8466,#6955,#6956);
#5673=AXIS2_PLACEMENT_3D('',#8467,#6957,#6958);
#5674=AXIS2_PLACEMENT_3D('',#8469,#6959,#6960);
#5675=AXIS2_PLACEMENT_3D('',#8470,#6961,#6962);
#5676=AXIS2_PLACEMENT_3D('',#8472,#6963,#6964);
#5677=AXIS2_PLACEMENT_3D('',#8474,#6966,#6967);
#5678=AXIS2_PLACEMENT_3D('',#8476,#6968,#6969);
#5679=AXIS2_PLACEMENT_3D('',#8479,#6971,#6972);
#5680=AXIS2_PLACEMENT_3D('',#8480,#6973,#6974);
#5681=AXIS2_PLACEMENT_3D('',#8481,#6975,#6976);
#5682=AXIS2_PLACEMENT_3D('',#8482,#6977,#6978);
#5683=AXIS2_PLACEMENT_3D('',#8483,#6979,#6980);
#5684=AXIS2_PLACEMENT_3D('',#8484,#6981,#6982);
#5685=AXIS2_PLACEMENT_3D('',#8487,#6983,#6984);
#5686=AXIS2_PLACEMENT_3D('',#8488,#6985,#6986);
#5687=AXIS2_PLACEMENT_3D('',#8490,#6987,#6988);
#5688=AXIS2_PLACEMENT_3D('',#8492,#6989,#6990);
#5689=AXIS2_PLACEMENT_3D('',#8493,#6991,#6992);
#5690=AXIS2_PLACEMENT_3D('',#8494,#6993,#6994);
#5691=AXIS2_PLACEMENT_3D('',#8497,#6996,#6997);
#5692=AXIS2_PLACEMENT_3D('',#8498,#6998,#6999);
#5693=AXIS2_PLACEMENT_3D('',#8500,#7000,#7001);
#5694=AXIS2_PLACEMENT_3D('',#8503,#7003,#7004);
#5695=AXIS2_PLACEMENT_3D('',#8504,#7005,#7006);
#5696=AXIS2_PLACEMENT_3D('',#8507,#7008,#7009);
#5697=AXIS2_PLACEMENT_3D('',#8508,#7010,#7011);
#5698=AXIS2_PLACEMENT_3D('',#8509,#7012,#7013);
#5699=AXIS2_PLACEMENT_3D('',#8511,#7014,#7015);
#5700=AXIS2_PLACEMENT_3D('',#8513,#7017,#7018);
#5701=AXIS2_PLACEMENT_3D('',#8515,#7019,#7020);
#5702=AXIS2_PLACEMENT_3D('',#8516,#7021,#7022);
#5703=AXIS2_PLACEMENT_3D('',#8518,#7024,#7025);
#5704=AXIS2_PLACEMENT_3D('',#8519,#7026,#7027);
#5705=AXIS2_PLACEMENT_3D('',#8522,#7028,#7029);
#5706=AXIS2_PLACEMENT_3D('',#8523,#7030,#7031);
#5707=AXIS2_PLACEMENT_3D('',#8525,#7032,#7033);
#5708=AXIS2_PLACEMENT_3D('',#8527,#7034,#7035);
#5709=AXIS2_PLACEMENT_3D('',#8528,#7036,#7037);
#5710=AXIS2_PLACEMENT_3D('',#8529,#7038,#7039);
#5711=AXIS2_PLACEMENT_3D('',#8531,#7040,#7041);
#5712=AXIS2_PLACEMENT_3D('',#8533,#7043,#7044);
#5713=AXIS2_PLACEMENT_3D('',#8535,#7045,#7046);
#5714=AXIS2_PLACEMENT_3D('',#8537,#7047,#7048);
#5715=AXIS2_PLACEMENT_3D('',#8538,#7049,#7050);
#5716=AXIS2_PLACEMENT_3D('',#8540,#7051,#7052);
#5717=AXIS2_PLACEMENT_3D('',#8542,#7054,#7055);
#5718=AXIS2_PLACEMENT_3D('',#8544,#7056,#7057);
#5719=AXIS2_PLACEMENT_3D('',#8546,#7059,#7060);
#5720=AXIS2_PLACEMENT_3D('',#8548,#7061,#7062);
#5721=AXIS2_PLACEMENT_3D('',#8550,#7064,#7065);
#5722=AXIS2_PLACEMENT_3D('',#8551,#7066,#7067);
#5723=AXIS2_PLACEMENT_3D('',#8553,#7069,#7070);
#5724=AXIS2_PLACEMENT_3D('',#8554,#7071,#7072);
#5725=AXIS2_PLACEMENT_3D('',#8557,#7073,#7074);
#5726=AXIS2_PLACEMENT_3D('',#8558,#7075,#7076);
#5727=AXIS2_PLACEMENT_3D('',#8561,#7077,#7078);
#5728=AXIS2_PLACEMENT_3D('',#8562,#7079,#7080);
#5729=AXIS2_PLACEMENT_3D('',#8565,#7081,#7082);
#5730=AXIS2_PLACEMENT_3D('',#8566,#7083,#7084);
#5731=AXIS2_PLACEMENT_3D('',#8569,#7085,#7086);
#5732=AXIS2_PLACEMENT_3D('',#8570,#7087,#7088);
#5733=AXIS2_PLACEMENT_3D('',#8573,#7089,#7090);
#5734=AXIS2_PLACEMENT_3D('',#8574,#7091,#7092);
#5735=AXIS2_PLACEMENT_3D('',#8577,#7093,#7094);
#5736=AXIS2_PLACEMENT_3D('',#8578,#7095,#7096);
#5737=AXIS2_PLACEMENT_3D('',#8581,#7097,#7098);
#5738=AXIS2_PLACEMENT_3D('',#8582,#7099,#7100);
#5739=AXIS2_PLACEMENT_3D('',#8585,#7101,#7102);
#5740=AXIS2_PLACEMENT_3D('',#8586,#7103,#7104);
#5741=AXIS2_PLACEMENT_3D('',#8587,#7105,#7106);
#5742=AXIS2_PLACEMENT_3D('',#8613,#7107,#7108);
#5743=AXIS2_PLACEMENT_3D('',#8637,#7109,#7110);
#5744=AXIS2_PLACEMENT_3D('',#8638,#7111,#7112);
#5745=AXIS2_PLACEMENT_3D('',#8640,#7113,#7114);
#5746=AXIS2_PLACEMENT_3D('',#8665,#7115,#7116);
#5747=AXIS2_PLACEMENT_3D('',#8690,#7117,#7118);
#5748=AXIS2_PLACEMENT_3D('',#8706,#7120,#7121);
#5749=AXIS2_PLACEMENT_3D('',#8721,#7122,#7123);
#5750=AXIS2_PLACEMENT_3D('',#8746,#7124,#7125);
#5751=AXIS2_PLACEMENT_3D('',#8771,#7126,#7127);
#5752=AXIS2_PLACEMENT_3D('',#8796,#7128,#7129);
#5753=AXIS2_PLACEMENT_3D('',#8820,#7130,#7131);
#5754=AXIS2_PLACEMENT_3D('',#8821,#7132,#7133);
#5755=AXIS2_PLACEMENT_3D('',#8823,#7134,#7135);
#5756=AXIS2_PLACEMENT_3D('',#8824,#7136,#7137);
#5757=AXIS2_PLACEMENT_3D('',#8825,#7138,#7139);
#5758=AXIS2_PLACEMENT_3D('',#8849,#7140,#7141);
#5759=AXIS2_PLACEMENT_3D('',#8850,#7142,#7143);
#5760=AXIS2_PLACEMENT_3D('',#8852,#7144,#7145);
#5761=AXIS2_PLACEMENT_3D('',#8853,#7146,#7147);
#5762=AXIS2_PLACEMENT_3D('',#8854,#7148,#7149);
#5763=AXIS2_PLACEMENT_3D('',#8878,#7150,#7151);
#5764=AXIS2_PLACEMENT_3D('',#8879,#7152,#7153);
#5765=AXIS2_PLACEMENT_3D('',#8881,#7154,#7155);
#5766=AXIS2_PLACEMENT_3D('',#8882,#7156,#7157);
#5767=AXIS2_PLACEMENT_3D('',#8883,#7158,#7159);
#5768=AXIS2_PLACEMENT_3D('',#8898,#7160,#7161);
#5769=AXIS2_PLACEMENT_3D('',#8911,#7162,#7163);
#5770=AXIS2_PLACEMENT_3D('',#8913,#7164,#7165);
#5771=AXIS2_PLACEMENT_3D('',#8914,#7166,#7167);
#5772=AXIS2_PLACEMENT_3D('',#8915,#7168,#7169);
#5773=AXIS2_PLACEMENT_3D('',#8939,#7170,#7171);
#5774=AXIS2_PLACEMENT_3D('',#8940,#7172,#7173);
#5775=AXIS2_PLACEMENT_3D('',#8942,#7174,#7175);
#5776=AXIS2_PLACEMENT_3D('',#8943,#7176,#7177);
#5777=AXIS2_PLACEMENT_3D('',#8944,#7178,#7179);
#5778=AXIS2_PLACEMENT_3D('',#8968,#7180,#7181);
#5779=AXIS2_PLACEMENT_3D('',#8969,#7182,#7183);
#5780=AXIS2_PLACEMENT_3D('',#8971,#7184,#7185);
#5781=AXIS2_PLACEMENT_3D('',#8972,#7186,#7187);
#5782=AXIS2_PLACEMENT_3D('',#8973,#7188,#7189);
#5783=AXIS2_PLACEMENT_3D('',#8997,#7190,#7191);
#5784=AXIS2_PLACEMENT_3D('',#8998,#7192,#7193);
#5785=AXIS2_PLACEMENT_3D('',#9000,#7194,#7195);
#5786=AXIS2_PLACEMENT_3D('',#9003,#7197,#7198);
#5787=AXIS2_PLACEMENT_3D('',#9027,#7199,#7200);
#5788=AXIS2_PLACEMENT_3D('',#9028,#7201,#7202);
#5789=AXIS2_PLACEMENT_3D('',#9029,#7203,#7204);
#5790=AXIS2_PLACEMENT_3D('',#9030,#7205,#7206);
#5791=AXIS2_PLACEMENT_3D('',#9031,#7207,#7208);
#5792=AXIS2_PLACEMENT_3D('',#9032,#7209,#7210);
#5793=AXIS2_PLACEMENT_3D('',#9033,#7211,#7212);
#5794=AXIS2_PLACEMENT_3D('',#9034,#7213,#7214);
#5795=AXIS2_PLACEMENT_3D('',#9035,#7215,#7216);
#5796=AXIS2_PLACEMENT_3D('',#9037,#7217,#7218);
#5797=AXIS2_PLACEMENT_3D('',#9039,#7219,#7220);
#5798=AXIS2_PLACEMENT_3D('',#9040,#7221,#7222);
#5799=AXIS2_PLACEMENT_3D('',#9042,#7223,#7224);
#5800=AXIS2_PLACEMENT_3D('',#9044,#7226,#7227);
#5801=AXIS2_PLACEMENT_3D('',#9046,#7228,#7229);
#5802=AXIS2_PLACEMENT_3D('',#9047,#7230,#7231);
#5803=AXIS2_PLACEMENT_3D('',#9049,#7233,#7234);
#5804=AXIS2_PLACEMENT_3D('',#9051,#7235,#7236);
#5805=AXIS2_PLACEMENT_3D('',#9053,#7237,#7238);
#5806=AXIS2_PLACEMENT_3D('',#9054,#7239,#7240);
#5807=AXIS2_PLACEMENT_3D('',#9056,#7241,#7242);
#5808=AXIS2_PLACEMENT_3D('',#9058,#7244,#7245);
#5809=AXIS2_PLACEMENT_3D('',#9060,#7246,#7247);
#5810=AXIS2_PLACEMENT_3D('',#9061,#7248,#7249);
#5811=AXIS2_PLACEMENT_3D('',#9063,#7251,#7252);
#5812=AXIS2_PLACEMENT_3D('',#9064,#7253,#7254);
#5813=AXIS2_PLACEMENT_3D('',#9065,#7255,#7256);
#5814=AXIS2_PLACEMENT_3D('',#9066,#7257,#7258);
#5815=AXIS2_PLACEMENT_3D('',#9067,#7259,#7260);
#5816=AXIS2_PLACEMENT_3D('',#9068,#7261,#7262);
#5817=AXIS2_PLACEMENT_3D('',#9069,#7263,#7264);
#5818=AXIS2_PLACEMENT_3D('',#9078,#7269,#7270);
#5819=AXIS2_PLACEMENT_3D('',#9084,#7274,#7275);
#5820=AXIS2_PLACEMENT_3D('',#9090,#7279,#7280);
#5821=AXIS2_PLACEMENT_3D('',#9096,#7284,#7285);
#5822=AXIS2_PLACEMENT_3D('',#9102,#7289,#7290);
#5823=AXIS2_PLACEMENT_3D('',#9105,#7293,#7294);
#5824=AXIS2_PLACEMENT_3D('',#9106,#7295,#7296);
#5825=AXIS2_PLACEMENT_3D('',#9107,#7297,#7298);
#5826=AXIS2_PLACEMENT_3D('',#9109,#7299,#7300);
#5827=AXIS2_PLACEMENT_3D('',#9110,#7301,#7302);
#5828=AXIS2_PLACEMENT_3D('',#9112,#7303,#7304);
#5829=AXIS2_PLACEMENT_3D('',#9113,#7305,#7306);
#5830=AXIS2_PLACEMENT_3D('',#9115,#7307,#7308);
#5831=AXIS2_PLACEMENT_3D('',#9117,#7310,#7311);
#5832=AXIS2_PLACEMENT_3D('',#9119,#7312,#7313);
#5833=AXIS2_PLACEMENT_3D('',#9121,#7315,#7316);
#5834=AXIS2_PLACEMENT_3D('',#9123,#7317,#7318);
#5835=AXIS2_PLACEMENT_3D('',#9125,#7320,#7321);
#5836=AXIS2_PLACEMENT_3D('',#9127,#7322,#7323);
#5837=AXIS2_PLACEMENT_3D('',#9128,#7324,#7325);
#5838=AXIS2_PLACEMENT_3D('',#9130,#7326,#7327);
#5839=AXIS2_PLACEMENT_3D('',#9132,#7329,#7330);
#5840=AXIS2_PLACEMENT_3D('',#9134,#7332,#7333);
#5841=AXIS2_PLACEMENT_3D('',#9135,#7334,#7335);
#5842=AXIS2_PLACEMENT_3D('',#9136,#7336,#7337);
#5843=AXIS2_PLACEMENT_3D('',#9137,#7338,#7339);
#5844=AXIS2_PLACEMENT_3D('',#9138,#7340,#7341);
#5845=AXIS2_PLACEMENT_3D('',#9139,#7342,#7343);
#5846=AXIS2_PLACEMENT_3D('',#9140,#7344,#7345);
#5847=AXIS2_PLACEMENT_3D('',#9141,#7346,#7347);
#5848=AXIS2_PLACEMENT_3D('',#9142,#7348,#7349);
#5849=AXIS2_PLACEMENT_3D('',#9143,#7350,#7351);
#5850=AXIS2_PLACEMENT_3D('',#9144,#7352,#7353);
#5851=AXIS2_PLACEMENT_3D('',#9145,#7354,#7355);
#5852=AXIS2_PLACEMENT_3D('',#9146,#7356,#7357);
#5853=AXIS2_PLACEMENT_3D('',#9147,#7358,#7359);
#5854=AXIS2_PLACEMENT_3D('',#9148,#7360,#7361);
#5855=AXIS2_PLACEMENT_3D('',#9149,#7362,#7363);
#5856=AXIS2_PLACEMENT_3D('',#9150,#7364,#7365);
#5857=AXIS2_PLACEMENT_3D('',#9152,#7366,#7367);
#5858=AXIS2_PLACEMENT_3D('',#9154,#7368,#7369);
#5859=AXIS2_PLACEMENT_3D('',#9155,#7370,#7371);
#5860=AXIS2_PLACEMENT_3D('',#9157,#7372,#7373);
#5861=AXIS2_PLACEMENT_3D('',#9159,#7374,#7375);
#5862=AXIS2_PLACEMENT_3D('',#9160,#7376,#7377);
#5863=AXIS2_PLACEMENT_3D('',#9162,#7379,#7380);
#5864=AXIS2_PLACEMENT_3D('',#9166,#7382,#7383);
#5865=AXIS2_PLACEMENT_3D('',#9168,#7384,#7385);
#5866=AXIS2_PLACEMENT_3D('',#9169,#7386,#7387);
#5867=AXIS2_PLACEMENT_3D('',#9170,#7388,#7389);
#5868=AXIS2_PLACEMENT_3D('',#9172,#7390,#7391);
#5869=AXIS2_PLACEMENT_3D('',#9174,#7393,#7394);
#5870=AXIS2_PLACEMENT_3D('',#9175,#7395,#7396);
#5871=AXIS2_PLACEMENT_3D('',#9181,#7400,#7401);
#5872=AXIS2_PLACEMENT_3D('',#9187,#7405,#7406);
#5873=AXIS2_PLACEMENT_3D('',#9193,#7410,#7411);
#5874=AXIS2_PLACEMENT_3D('',#9202,#7416,#7417);
#5875=AXIS2_PLACEMENT_3D('',#9205,#7419,#7420);
#5876=AXIS2_PLACEMENT_3D('',#9208,#7422,#7423);
#5877=AXIS2_PLACEMENT_3D('',#9209,#7424,#7425);
#5878=AXIS2_PLACEMENT_3D('',#9211,#7426,#7427);
#5879=AXIS2_PLACEMENT_3D('',#9213,#7429,#7430);
#5880=AXIS2_PLACEMENT_3D('',#9216,#7432,#7433);
#5881=AXIS2_PLACEMENT_3D('',#9218,#7435,#7436);
#5882=AXIS2_PLACEMENT_3D('',#9219,#7437,#7438);
#5883=AXIS2_PLACEMENT_3D('',#9221,#7440,#7441);
#5884=AXIS2_PLACEMENT_3D('',#9222,#7442,#7443);
#5885=AXIS2_PLACEMENT_3D('',#9223,#7444,#7445);
#5886=AXIS2_PLACEMENT_3D('',#9225,#7446,#7447);
#5887=AXIS2_PLACEMENT_3D('',#9228,#7449,#7450);
#5888=AXIS2_PLACEMENT_3D('',#9229,#7451,#7452);
#5889=AXIS2_PLACEMENT_3D('',#9231,#7453,#7454);
#5890=AXIS2_PLACEMENT_3D('',#9234,#7456,#7457);
#5891=AXIS2_PLACEMENT_3D('',#9235,#7458,#7459);
#5892=AXIS2_PLACEMENT_3D('',#9236,#7460,#7461);
#5893=AXIS2_PLACEMENT_3D('',#9237,#7462,#7463);
#5894=AXIS2_PLACEMENT_3D('',#9238,#7464,#7465);
#5895=AXIS2_PLACEMENT_3D('',#9240,#7466,#7467);
#5896=AXIS2_PLACEMENT_3D('',#9243,#7469,#7470);
#5897=AXIS2_PLACEMENT_3D('',#9244,#7471,#7472);
#5898=AXIS2_PLACEMENT_3D('',#9253,#7477,#7478);
#5899=AXIS2_PLACEMENT_3D('',#9259,#7482,#7483);
#5900=AXIS2_PLACEMENT_3D('',#9265,#7487,#7488);
#5901=AXIS2_PLACEMENT_3D('',#9271,#7492,#7493);
#5902=AXIS2_PLACEMENT_3D('',#9277,#7497,#7498);
#5903=AXIS2_PLACEMENT_3D('',#9280,#7501,#7502);
#5904=AXIS2_PLACEMENT_3D('',#9281,#7503,#7504);
#5905=AXIS2_PLACEMENT_3D('',#9282,#7505,#7506);
#5906=AXIS2_PLACEMENT_3D('',#9283,#7507,#7508);
#5907=AXIS2_PLACEMENT_3D('',#9284,#7509,#7510);
#5908=AXIS2_PLACEMENT_3D('',#9285,#7511,#7512);
#5909=AXIS2_PLACEMENT_3D('',#9286,#7513,#7514);
#5910=AXIS2_PLACEMENT_3D('',#9287,#7515,#7516);
#5911=AXIS2_PLACEMENT_3D('',#9289,#7517,#7518);
#5912=AXIS2_PLACEMENT_3D('',#9292,#7520,#7521);
#5913=AXIS2_PLACEMENT_3D('',#9293,#7522,#7523);
#5914=AXIS2_PLACEMENT_3D('',#9295,#7524,#7525);
#5915=AXIS2_PLACEMENT_3D('',#9298,#7527,#7528);
#5916=AXIS2_PLACEMENT_3D('',#9299,#7529,#7530);
#5917=AXIS2_PLACEMENT_3D('',#9304,#7532,#7533);
#5918=AXIS2_PLACEMENT_3D('',#9307,#7535,#7536);
#5919=AXIS2_PLACEMENT_3D('',#9308,#7537,#7538);
#5920=AXIS2_PLACEMENT_3D('',#9309,#7539,#7540);
#5921=AXIS2_PLACEMENT_3D('',#9310,#7541,#7542);
#5922=AXIS2_PLACEMENT_3D('',#9311,#7543,#7544);
#5923=AXIS2_PLACEMENT_3D('',#9312,#7545,#7546);
#5924=AXIS2_PLACEMENT_3D('',#9313,#7547,#7548);
#5925=AXIS2_PLACEMENT_3D('',#9314,#7549,#7550);
#5926=AXIS2_PLACEMENT_3D('',#9315,#7551,#7552);
#5927=AXIS2_PLACEMENT_3D('',#9316,#7553,#7554);
#5928=AXIS2_PLACEMENT_3D('',#9317,#7555,#7556);
#5929=DIRECTION('axis',(0.,0.,1.));
#5930=DIRECTION('refdir',(1.,0.,0.));
#5931=DIRECTION('axis',(0.,0.,1.));
#5932=DIRECTION('refdir',(1.,0.,0.));
#5933=DIRECTION('axis',(0.,0.,1.));
#5934=DIRECTION('refdir',(1.,0.,0.));
#5935=DIRECTION('center_axis',(0.,1.,0.));
#5936=DIRECTION('ref_axis',(1.,0.,0.));
#5937=DIRECTION('center_axis',(0.,1.,0.));
#5938=DIRECTION('ref_axis',(1.,0.,0.));
#5939=DIRECTION('center_axis',(0.,1.,0.));
#5940=DIRECTION('ref_axis',(1.,0.,0.));
#5941=DIRECTION('center_axis',(0.,1.,0.));
#5942=DIRECTION('ref_axis',(1.,0.,0.));
#5943=DIRECTION('center_axis',(0.,1.,0.));
#5944=DIRECTION('ref_axis',(1.,0.,0.));
#5945=DIRECTION('center_axis',(0.,1.,0.));
#5946=DIRECTION('ref_axis',(1.,0.,0.));
#5947=DIRECTION('center_axis',(0.,1.,0.));
#5948=DIRECTION('ref_axis',(1.,0.,0.));
#5949=DIRECTION('center_axis',(0.,1.,0.));
#5950=DIRECTION('ref_axis',(1.,0.,0.));
#5951=DIRECTION('center_axis',(0.,1.,0.));
#5952=DIRECTION('ref_axis',(1.,0.,0.));
#5953=DIRECTION('center_axis',(0.,-1.,0.));
#5954=DIRECTION('ref_axis',(1.,0.,0.));
#5955=DIRECTION('center_axis',(0.,1.,0.));
#5956=DIRECTION('ref_axis',(1.,0.,0.));
#5957=DIRECTION('',(0.,1.,0.));
#5958=DIRECTION('',(0.,-1.,0.));
#5959=DIRECTION('center_axis',(0.,-1.,0.));
#5960=DIRECTION('ref_axis',(1.,0.,0.));
#5961=DIRECTION('center_axis',(0.,1.,0.));
#5962=DIRECTION('ref_axis',(1.,0.,0.));
#5963=DIRECTION('',(0.,-1.,0.));
#5964=DIRECTION('center_axis',(0.,-1.,0.));
#5965=DIRECTION('ref_axis',(1.,0.,0.));
#5966=DIRECTION('',(0.,1.,0.));
#5967=DIRECTION('center_axis',(0.,1.,0.));
#5968=DIRECTION('ref_axis',(1.,0.,0.));
#5969=DIRECTION('',(0.,1.,0.));
#5970=DIRECTION('',(0.,-1.,0.));
#5971=DIRECTION('center_axis',(0.,-1.,0.));
#5972=DIRECTION('ref_axis',(1.,0.,0.));
#5973=DIRECTION('center_axis',(0.,1.,0.));
#5974=DIRECTION('ref_axis',(1.,0.,0.));
#5975=DIRECTION('',(0.,1.,0.));
#5976=DIRECTION('center_axis',(0.,1.,0.));
#5977=DIRECTION('ref_axis',(1.,0.,0.));
#5978=DIRECTION('center_axis',(0.,1.,0.));
#5979=DIRECTION('ref_axis',(-1.,0.,-1.22464679914735E-16));
#5980=DIRECTION('',(0.,-1.,0.));
#5981=DIRECTION('center_axis',(0.,-1.,0.));
#5982=DIRECTION('ref_axis',(1.,0.,0.));
#5983=DIRECTION('',(0.,1.,0.));
#5984=DIRECTION('center_axis',(0.,1.,0.));
#5985=DIRECTION('ref_axis',(1.,0.,0.));
#5986=DIRECTION('center_axis',(0.,1.,0.));
#5987=DIRECTION('ref_axis',(1.,0.,0.));
#5988=DIRECTION('',(0.,1.,0.));
#5989=DIRECTION('center_axis',(0.,-1.,0.));
#5990=DIRECTION('ref_axis',(1.,0.,0.));
#5991=DIRECTION('center_axis',(0.,-1.,0.));
#5992=DIRECTION('ref_axis',(1.,0.,0.));
#5993=DIRECTION('center_axis',(0.,1.,0.));
#5994=DIRECTION('ref_axis',(1.,0.,0.));
#5995=DIRECTION('center_axis',(0.,1.,0.));
#5996=DIRECTION('ref_axis',(1.,0.,0.));
#5997=DIRECTION('',(0.,1.,0.));
#5998=DIRECTION('center_axis',(0.,-1.,0.));
#5999=DIRECTION('ref_axis',(1.,0.,0.));
#6000=DIRECTION('center_axis',(0.,-1.,0.));
#6001=DIRECTION('ref_axis',(1.,0.,0.));
#6002=DIRECTION('center_axis',(0.,1.,0.));
#6003=DIRECTION('ref_axis',(1.,0.,0.));
#6004=DIRECTION('center_axis',(0.,1.,0.));
#6005=DIRECTION('ref_axis',(1.,0.,0.));
#6006=DIRECTION('',(0.,1.,0.));
#6007=DIRECTION('center_axis',(0.,-1.,0.));
#6008=DIRECTION('ref_axis',(1.,0.,0.));
#6009=DIRECTION('center_axis',(0.,-1.,0.));
#6010=DIRECTION('ref_axis',(1.,0.,0.));
#6011=DIRECTION('center_axis',(0.,1.,0.));
#6012=DIRECTION('ref_axis',(0.,0.,1.));
#6013=DIRECTION('center_axis',(0.,-1.,0.));
#6014=DIRECTION('ref_axis',(1.,0.,0.));
#6015=DIRECTION('center_axis',(0.,1.,0.));
#6016=DIRECTION('ref_axis',(1.,0.,0.));
#6017=DIRECTION('center_axis',(0.,1.,0.));
#6018=DIRECTION('ref_axis',(1.,0.,0.));
#6019=DIRECTION('',(0.,1.,0.));
#6020=DIRECTION('center_axis',(0.,-1.,0.));
#6021=DIRECTION('ref_axis',(1.,0.,0.));
#6022=DIRECTION('center_axis',(0.,-1.,0.));
#6023=DIRECTION('ref_axis',(1.,0.,0.));
#6024=DIRECTION('center_axis',(0.,1.,0.));
#6025=DIRECTION('ref_axis',(1.,0.,0.));
#6026=DIRECTION('center_axis',(0.,1.,0.));
#6027=DIRECTION('ref_axis',(1.,0.,0.));
#6028=DIRECTION('',(0.,1.,0.));
#6029=DIRECTION('center_axis',(0.,-1.,0.));
#6030=DIRECTION('ref_axis',(1.,0.,0.));
#6031=DIRECTION('center_axis',(0.,1.,0.));
#6032=DIRECTION('ref_axis',(1.,0.,0.));
#6033=DIRECTION('center_axis',(0.,1.,0.));
#6034=DIRECTION('ref_axis',(1.,0.,0.));
#6035=DIRECTION('',(0.,1.,0.));
#6036=DIRECTION('center_axis',(0.,-1.,0.));
#6037=DIRECTION('ref_axis',(1.,0.,0.));
#6038=DIRECTION('center_axis',(0.,1.,0.));
#6039=DIRECTION('ref_axis',(1.,0.,0.));
#6040=DIRECTION('center_axis',(0.,1.,0.));
#6041=DIRECTION('ref_axis',(1.,0.,0.));
#6042=DIRECTION('',(0.,1.,0.));
#6043=DIRECTION('center_axis',(0.,-1.,0.));
#6044=DIRECTION('ref_axis',(1.,0.,0.));
#6045=DIRECTION('center_axis',(0.,1.,0.));
#6046=DIRECTION('ref_axis',(1.,0.,0.));
#6047=DIRECTION('center_axis',(0.,1.,0.));
#6048=DIRECTION('ref_axis',(1.,0.,0.));
#6049=DIRECTION('',(0.,1.,0.));
#6050=DIRECTION('center_axis',(-0.832050294337844,0.,-0.554700196225229));
#6051=DIRECTION('ref_axis',(-0.554700196225229,0.,0.832050294337844));
#6052=DIRECTION('',(0.554700196225229,0.,-0.832050294337844));
#6053=DIRECTION('',(0.,1.,0.));
#6054=DIRECTION('',(-0.554700196225229,0.,0.832050294337844));
#6055=DIRECTION('',(0.,1.,0.));
#6056=DIRECTION('center_axis',(0.,0.,-1.));
#6057=DIRECTION('ref_axis',(-1.,0.,0.));
#6058=DIRECTION('',(1.,0.,0.));
#6059=DIRECTION('',(-1.,0.,0.));
#6060=DIRECTION('',(0.,1.,0.));
#6061=DIRECTION('center_axis',(0.832050294337844,0.,-0.554700196225229));
#6062=DIRECTION('ref_axis',(-0.554700196225229,0.,-0.832050294337844));
#6063=DIRECTION('',(0.554700196225229,0.,0.832050294337844));
#6064=DIRECTION('',(-0.554700196225229,0.,-0.832050294337844));
#6065=DIRECTION('',(0.,1.,0.));
#6066=DIRECTION('center_axis',(1.,0.,0.));
#6067=DIRECTION('ref_axis',(0.,0.,-1.));
#6068=DIRECTION('',(0.,0.,1.));
#6069=DIRECTION('',(0.,0.,-1.));
#6070=DIRECTION('',(0.,1.,0.));
#6071=DIRECTION('center_axis',(0.894427190999916,0.,0.447213595499958));
#6072=DIRECTION('ref_axis',(0.447213595499958,0.,-0.894427190999916));
#6073=DIRECTION('',(-0.447213595499958,0.,0.894427190999916));
#6074=DIRECTION('',(0.447213595499958,0.,-0.894427190999916));
#6075=DIRECTION('',(0.,1.,0.));
#6076=DIRECTION('center_axis',(0.,0.,1.));
#6077=DIRECTION('ref_axis',(1.,0.,0.));
#6078=DIRECTION('',(-1.,0.,0.));
#6079=DIRECTION('',(1.,0.,0.));
#6080=DIRECTION('',(0.,1.,0.));
#6081=DIRECTION('center_axis',(-0.894427190999916,0.,0.447213595499958));
#6082=DIRECTION('ref_axis',(0.447213595499958,0.,0.894427190999916));
#6083=DIRECTION('',(-0.447213595499958,0.,-0.894427190999916));
#6084=DIRECTION('',(0.447213595499958,0.,0.894427190999916));
#6085=DIRECTION('',(0.,1.,0.));
#6086=DIRECTION('center_axis',(-1.,0.,0.));
#6087=DIRECTION('ref_axis',(0.,0.,1.));
#6088=DIRECTION('',(0.,0.,-1.));
#6089=DIRECTION('',(0.,0.,1.));
#6090=DIRECTION('center_axis',(0.,1.,0.));
#6091=DIRECTION('ref_axis',(0.,0.,1.));
#6092=DIRECTION('center_axis',(0.,1.,0.));
#6093=DIRECTION('ref_axis',(1.,0.,0.));
#6094=DIRECTION('axis',(0.,0.,1.));
#6095=DIRECTION('refdir',(1.,0.,0.));
#6096=DIRECTION('center_axis',(0.,1.,0.));
#6097=DIRECTION('ref_axis',(1.,0.,0.));
#6098=DIRECTION('center_axis',(0.,-1.,0.));
#6099=DIRECTION('ref_axis',(1.,0.,0.));
#6100=DIRECTION('center_axis',(0.,1.,0.));
#6101=DIRECTION('ref_axis',(1.,0.,0.));
#6102=DIRECTION('center_axis',(0.,-1.,0.));
#6103=DIRECTION('ref_axis',(1.,0.,0.));
#6104=DIRECTION('center_axis',(0.,1.,0.));
#6105=DIRECTION('ref_axis',(1.,0.,0.));
#6106=DIRECTION('center_axis',(0.,-1.,0.));
#6107=DIRECTION('ref_axis',(1.,0.,0.));
#6108=DIRECTION('center_axis',(0.,1.,0.));
#6109=DIRECTION('ref_axis',(1.,0.,0.));
#6110=DIRECTION('center_axis',(0.,-1.,0.));
#6111=DIRECTION('ref_axis',(1.,0.,0.));
#6112=DIRECTION('center_axis',(0.,1.,0.));
#6113=DIRECTION('ref_axis',(1.,0.,0.));
#6114=DIRECTION('center_axis',(0.,-1.,0.));
#6115=DIRECTION('ref_axis',(1.,0.,0.));
#6116=DIRECTION('center_axis',(0.,1.,0.));
#6117=DIRECTION('ref_axis',(1.,0.,0.));
#6118=DIRECTION('',(0.,-1.,0.));
#6119=DIRECTION('',(0.,1.,0.));
#6120=DIRECTION('center_axis',(0.,1.,0.));
#6121=DIRECTION('ref_axis',(1.,0.,0.));
#6122=DIRECTION('center_axis',(0.,1.,0.));
#6123=DIRECTION('ref_axis',(-1.,0.,-1.22464679914735E-16));
#6124=DIRECTION('',(0.,-1.,0.));
#6125=DIRECTION('',(0.,1.,0.));
#6126=DIRECTION('center_axis',(0.,1.,0.));
#6127=DIRECTION('ref_axis',(1.,0.,0.));
#6128=DIRECTION('center_axis',(0.,1.,0.));
#6129=DIRECTION('ref_axis',(1.,0.,0.));
#6130=DIRECTION('',(0.,1.,0.));
#6131=DIRECTION('center_axis',(0.,1.,0.));
#6132=DIRECTION('ref_axis',(1.,0.,0.));
#6133=DIRECTION('',(0.,-1.,0.));
#6134=DIRECTION('center_axis',(0.,1.,0.));
#6135=DIRECTION('ref_axis',(1.,0.,0.));
#6136=DIRECTION('center_axis',(0.,-1.,0.));
#6137=DIRECTION('ref_axis',(1.,0.,0.));
#6138=DIRECTION('',(0.,1.,0.));
#6139=DIRECTION('center_axis',(0.,1.,0.));
#6140=DIRECTION('ref_axis',(1.,0.,0.));
#6141=DIRECTION('',(0.,1.,0.));
#6142=DIRECTION('center_axis',(0.,1.,0.));
#6143=DIRECTION('ref_axis',(1.,0.,0.));
#6144=DIRECTION('',(0.,-1.,0.));
#6145=DIRECTION('center_axis',(0.,1.,0.));
#6146=DIRECTION('ref_axis',(1.,0.,0.));
#6147=DIRECTION('center_axis',(0.,1.,0.));
#6148=DIRECTION('ref_axis',(1.,0.,0.));
#6149=DIRECTION('',(0.,1.,0.));
#6150=DIRECTION('center_axis',(0.,-1.,0.));
#6151=DIRECTION('ref_axis',(1.,0.,0.));
#6152=DIRECTION('center_axis',(0.,1.,0.));
#6153=DIRECTION('ref_axis',(1.,0.,0.));
#6154=DIRECTION('center_axis',(0.,1.,0.));
#6155=DIRECTION('ref_axis',(1.,0.,0.));
#6156=DIRECTION('center_axis',(0.,1.,0.));
#6157=DIRECTION('ref_axis',(1.,0.,0.));
#6158=DIRECTION('',(0.,1.,0.));
#6159=DIRECTION('center_axis',(0.,-1.,0.));
#6160=DIRECTION('ref_axis',(1.,0.,0.));
#6161=DIRECTION('center_axis',(0.,1.,0.));
#6162=DIRECTION('ref_axis',(1.,0.,0.));
#6163=DIRECTION('center_axis',(0.,1.,0.));
#6164=DIRECTION('ref_axis',(1.,0.,0.));
#6165=DIRECTION('center_axis',(0.,1.,0.));
#6166=DIRECTION('ref_axis',(1.,0.,0.));
#6167=DIRECTION('center_axis',(0.,1.,0.));
#6168=DIRECTION('ref_axis',(1.,0.,0.));
#6169=DIRECTION('center_axis',(0.,1.,0.));
#6170=DIRECTION('ref_axis',(1.,0.,0.));
#6171=DIRECTION('',(0.,1.,0.));
#6172=DIRECTION('center_axis',(0.,-1.,0.));
#6173=DIRECTION('ref_axis',(1.,0.,0.));
#6174=DIRECTION('center_axis',(0.,1.,0.));
#6175=DIRECTION('ref_axis',(1.,0.,0.));
#6176=DIRECTION('center_axis',(0.,1.,0.));
#6177=DIRECTION('ref_axis',(1.,0.,0.));
#6178=DIRECTION('center_axis',(0.,1.,0.));
#6179=DIRECTION('ref_axis',(1.,0.,0.));
#6180=DIRECTION('',(0.,1.,0.));
#6181=DIRECTION('center_axis',(0.,-1.,0.));
#6182=DIRECTION('ref_axis',(1.,0.,0.));
#6183=DIRECTION('center_axis',(0.,1.,0.));
#6184=DIRECTION('ref_axis',(1.,0.,0.));
#6185=DIRECTION('center_axis',(0.,1.,0.));
#6186=DIRECTION('ref_axis',(1.,0.,0.));
#6187=DIRECTION('center_axis',(0.,1.,0.));
#6188=DIRECTION('ref_axis',(1.,0.,0.));
#6189=DIRECTION('',(0.,1.,0.));
#6190=DIRECTION('center_axis',(0.,-1.,0.));
#6191=DIRECTION('ref_axis',(1.,0.,0.));
#6192=DIRECTION('center_axis',(0.,1.,0.));
#6193=DIRECTION('ref_axis',(1.,0.,0.));
#6194=DIRECTION('center_axis',(0.,1.,0.));
#6195=DIRECTION('ref_axis',(1.,0.,0.));
#6196=DIRECTION('',(0.,1.,0.));
#6197=DIRECTION('center_axis',(0.,-1.,0.));
#6198=DIRECTION('ref_axis',(1.,0.,0.));
#6199=DIRECTION('center_axis',(0.,1.,0.));
#6200=DIRECTION('ref_axis',(1.,0.,0.));
#6201=DIRECTION('center_axis',(0.,1.,0.));
#6202=DIRECTION('ref_axis',(1.,0.,0.));
#6203=DIRECTION('',(0.,1.,0.));
#6204=DIRECTION('center_axis',(0.,-1.,0.));
#6205=DIRECTION('ref_axis',(1.,0.,0.));
#6206=DIRECTION('center_axis',(0.,1.,0.));
#6207=DIRECTION('ref_axis',(1.,0.,0.));
#6208=DIRECTION('',(0.,1.,0.));
#6209=DIRECTION('center_axis',(0.,-1.,0.));
#6210=DIRECTION('ref_axis',(1.,0.,0.));
#6211=DIRECTION('center_axis',(-0.832050294337844,0.,-0.554700196225229));
#6212=DIRECTION('ref_axis',(-0.554700196225229,0.,0.832050294337844));
#6213=DIRECTION('',(0.554700196225229,0.,-0.832050294337844));
#6214=DIRECTION('',(0.,1.,0.));
#6215=DIRECTION('',(-0.554700196225229,0.,0.832050294337844));
#6216=DIRECTION('',(0.,1.,0.));
#6217=DIRECTION('center_axis',(0.,0.,-1.));
#6218=DIRECTION('ref_axis',(-1.,0.,0.));
#6219=DIRECTION('',(1.,0.,0.));
#6220=DIRECTION('',(-1.,0.,0.));
#6221=DIRECTION('',(0.,1.,0.));
#6222=DIRECTION('center_axis',(0.832050294337844,0.,-0.554700196225229));
#6223=DIRECTION('ref_axis',(-0.554700196225229,0.,-0.832050294337844));
#6224=DIRECTION('',(0.554700196225229,0.,0.832050294337844));
#6225=DIRECTION('',(-0.554700196225229,0.,-0.832050294337844));
#6226=DIRECTION('',(0.,1.,0.));
#6227=DIRECTION('center_axis',(1.,0.,0.));
#6228=DIRECTION('ref_axis',(0.,0.,-1.));
#6229=DIRECTION('',(0.,0.,1.));
#6230=DIRECTION('',(0.,0.,-1.));
#6231=DIRECTION('',(0.,1.,0.));
#6232=DIRECTION('center_axis',(0.894427190999916,0.,0.447213595499958));
#6233=DIRECTION('ref_axis',(0.447213595499958,0.,-0.894427190999916));
#6234=DIRECTION('',(-0.447213595499958,0.,0.894427190999916));
#6235=DIRECTION('',(0.447213595499958,0.,-0.894427190999916));
#6236=DIRECTION('',(0.,1.,0.));
#6237=DIRECTION('center_axis',(0.,0.,1.));
#6238=DIRECTION('ref_axis',(1.,0.,0.));
#6239=DIRECTION('',(-1.,0.,0.));
#6240=DIRECTION('',(1.,0.,0.));
#6241=DIRECTION('',(0.,1.,0.));
#6242=DIRECTION('center_axis',(-0.894427190999916,0.,0.447213595499958));
#6243=DIRECTION('ref_axis',(0.447213595499958,0.,0.894427190999916));
#6244=DIRECTION('',(-0.447213595499958,0.,-0.894427190999916));
#6245=DIRECTION('',(0.447213595499958,0.,0.894427190999916));
#6246=DIRECTION('',(0.,1.,0.));
#6247=DIRECTION('center_axis',(-1.,0.,0.));
#6248=DIRECTION('ref_axis',(0.,0.,1.));
#6249=DIRECTION('',(0.,0.,-1.));
#6250=DIRECTION('',(0.,0.,1.));
#6251=DIRECTION('center_axis',(0.,1.,0.));
#6252=DIRECTION('ref_axis',(0.,0.,1.));
#6253=DIRECTION('center_axis',(0.,1.,0.));
#6254=DIRECTION('ref_axis',(1.,0.,0.));
#6255=DIRECTION('axis',(0.,0.,1.));
#6256=DIRECTION('refdir',(1.,0.,0.));
#6257=DIRECTION('center_axis',(0.,0.,1.));
#6258=DIRECTION('ref_axis',(1.,0.,0.));
#6259=DIRECTION('center_axis',(0.,0.,1.));
#6260=DIRECTION('ref_axis',(1.,0.,0.));
#6261=DIRECTION('',(0.,0.,1.));
#6262=DIRECTION('center_axis',(0.,0.,-1.));
#6263=DIRECTION('ref_axis',(1.,0.,0.));
#6264=DIRECTION('center_axis',(0.,1.,0.));
#6265=DIRECTION('ref_axis',(1.,0.,0.));
#6266=DIRECTION('center_axis',(0.,1.,0.));
#6267=DIRECTION('ref_axis',(1.,0.,0.));
#6268=DIRECTION('',(0.,1.,0.));
#6269=DIRECTION('center_axis',(0.,-1.,0.));
#6270=DIRECTION('ref_axis',(1.,0.,0.));
#6271=DIRECTION('center_axis',(0.,1.,0.));
#6272=DIRECTION('ref_axis',(1.,0.,0.));
#6273=DIRECTION('center_axis',(0.,1.,0.));
#6274=DIRECTION('ref_axis',(1.,0.,0.));
#6275=DIRECTION('',(0.,1.,0.));
#6276=DIRECTION('center_axis',(0.,-1.,0.));
#6277=DIRECTION('ref_axis',(1.,0.,0.));
#6278=DIRECTION('center_axis',(0.,1.,0.));
#6279=DIRECTION('ref_axis',(-1.,0.,0.));
#6280=DIRECTION('',(-1.,0.,0.));
#6281=DIRECTION('',(0.,0.,1.));
#6282=DIRECTION('',(-1.,0.,0.));
#6283=DIRECTION('',(0.,0.,1.));
#6284=DIRECTION('center_axis',(1.,0.,0.));
#6285=DIRECTION('ref_axis',(0.,1.,0.));
#6286=DIRECTION('',(0.,1.,0.));
#6287=DIRECTION('',(0.,1.,0.));
#6288=DIRECTION('',(0.,0.,1.));
#6289=DIRECTION('center_axis',(0.,-1.,0.));
#6290=DIRECTION('ref_axis',(1.,0.,0.));
#6291=DIRECTION('',(1.,0.,0.));
#6292=DIRECTION('',(1.,0.,0.));
#6293=DIRECTION('',(0.,0.,1.));
#6294=DIRECTION('center_axis',(-1.,0.,0.));
#6295=DIRECTION('ref_axis',(0.,-1.,0.));
#6296=DIRECTION('',(0.,-1.,0.));
#6297=DIRECTION('',(0.,-1.,0.));
#6298=DIRECTION('center_axis',(0.,0.,1.));
#6299=DIRECTION('ref_axis',(1.,0.,0.));
#6300=DIRECTION('center_axis',(0.,0.,1.));
#6301=DIRECTION('ref_axis',(1.,0.,0.));
#6302=DIRECTION('axis',(0.,0.,1.));
#6303=DIRECTION('refdir',(1.,0.,0.));
#6304=DIRECTION('center_axis',(0.,1.,0.));
#6305=DIRECTION('ref_axis',(1.,0.,0.));
#6306=DIRECTION('center_axis',(0.,-1.,0.));
#6307=DIRECTION('ref_axis',(1.,0.,0.));
#6308=DIRECTION('',(0.,-1.,0.));
#6309=DIRECTION('center_axis',(0.,-1.,0.));
#6310=DIRECTION('ref_axis',(1.,0.,0.));
#6311=DIRECTION('center_axis',(0.,1.,0.));
#6312=DIRECTION('ref_axis',(1.,0.,0.));
#6313=DIRECTION('center_axis',(0.,1.,0.));
#6314=DIRECTION('ref_axis',(1.,0.,0.));
#6315=DIRECTION('',(0.,-1.,0.));
#6316=DIRECTION('center_axis',(0.,1.,0.));
#6317=DIRECTION('ref_axis',(1.,0.,0.));
#6318=DIRECTION('center_axis',(0.,1.,0.));
#6319=DIRECTION('ref_axis',(1.,0.,0.));
#6320=DIRECTION('center_axis',(0.,1.,0.));
#6321=DIRECTION('ref_axis',(1.,0.,0.));
#6322=DIRECTION('axis',(0.,0.,1.));
#6323=DIRECTION('refdir',(1.,0.,0.));
#6324=DIRECTION('center_axis',(0.,1.,0.));
#6325=DIRECTION('ref_axis',(1.,0.,0.));
#6326=DIRECTION('center_axis',(0.,1.,0.));
#6327=DIRECTION('ref_axis',(1.,0.,0.));
#6328=DIRECTION('',(0.,1.,0.));
#6329=DIRECTION('center_axis',(0.,-1.,0.));
#6330=DIRECTION('ref_axis',(1.,0.,0.));
#6331=DIRECTION('center_axis',(0.,1.,0.));
#6332=DIRECTION('ref_axis',(1.,0.,0.));
#6333=DIRECTION('center_axis',(0.,1.,0.));
#6334=DIRECTION('ref_axis',(1.,0.,0.));
#6335=DIRECTION('center_axis',(0.,1.,0.));
#6336=DIRECTION('ref_axis',(1.,0.,0.));
#6337=DIRECTION('center_axis',(0.,1.,0.));
#6338=DIRECTION('ref_axis',(1.,0.,0.));
#6339=DIRECTION('center_axis',(0.,1.,0.));
#6340=DIRECTION('ref_axis',(1.,0.,0.));
#6341=DIRECTION('',(0.,-1.,0.));
#6342=DIRECTION('center_axis',(0.,1.,0.));
#6343=DIRECTION('ref_axis',(1.,0.,0.));
#6344=DIRECTION('center_axis',(0.,1.,0.));
#6345=DIRECTION('ref_axis',(1.,0.,0.));
#6346=DIRECTION('center_axis',(0.,1.,0.));
#6347=DIRECTION('ref_axis',(1.,0.,0.));
#6348=DIRECTION('center_axis',(0.,1.,0.));
#6349=DIRECTION('ref_axis',(1.,0.,0.));
#6350=DIRECTION('',(0.,-1.,0.));
#6351=DIRECTION('center_axis',(0.,1.,0.));
#6352=DIRECTION('ref_axis',(1.,0.,0.));
#6353=DIRECTION('axis',(0.,0.,1.));
#6354=DIRECTION('refdir',(1.,0.,0.));
#6355=DIRECTION('center_axis',(0.,1.,0.));
#6356=DIRECTION('ref_axis',(1.,0.,0.));
#6357=DIRECTION('center_axis',(0.,-1.,0.));
#6358=DIRECTION('ref_axis',(1.,0.,0.));
#6359=DIRECTION('',(0.,-1.,0.));
#6360=DIRECTION('center_axis',(0.,-1.,0.));
#6361=DIRECTION('ref_axis',(1.,0.,0.));
#6362=DIRECTION('center_axis',(0.,1.,0.));
#6363=DIRECTION('ref_axis',(1.,0.,0.));
#6364=DIRECTION('center_axis',(0.,1.,0.));
#6365=DIRECTION('ref_axis',(1.,0.,0.));
#6366=DIRECTION('',(0.,-1.,0.));
#6367=DIRECTION('center_axis',(0.,1.,0.));
#6368=DIRECTION('ref_axis',(1.,0.,0.));
#6369=DIRECTION('center_axis',(0.,1.,0.));
#6370=DIRECTION('ref_axis',(1.,0.,0.));
#6371=DIRECTION('center_axis',(0.,1.,0.));
#6372=DIRECTION('ref_axis',(1.,0.,0.));
#6373=DIRECTION('axis',(0.,0.,1.));
#6374=DIRECTION('refdir',(1.,0.,0.));
#6375=DIRECTION('center_axis',(0.,1.,0.));
#6376=DIRECTION('ref_axis',(1.,0.,0.));
#6377=DIRECTION('center_axis',(0.,-1.,0.));
#6378=DIRECTION('ref_axis',(1.,0.,0.));
#6379=DIRECTION('',(0.,-1.,0.));
#6380=DIRECTION('center_axis',(0.,-1.,0.));
#6381=DIRECTION('ref_axis',(1.,0.,0.));
#6382=DIRECTION('center_axis',(0.,1.,0.));
#6383=DIRECTION('ref_axis',(1.,0.,0.));
#6384=DIRECTION('center_axis',(0.,1.,0.));
#6385=DIRECTION('ref_axis',(1.,0.,0.));
#6386=DIRECTION('',(0.,-1.,0.));
#6387=DIRECTION('center_axis',(0.,1.,0.));
#6388=DIRECTION('ref_axis',(1.,0.,0.));
#6389=DIRECTION('center_axis',(0.,1.,0.));
#6390=DIRECTION('ref_axis',(1.,0.,0.));
#6391=DIRECTION('center_axis',(0.,1.,0.));
#6392=DIRECTION('ref_axis',(1.,0.,0.));
#6393=DIRECTION('axis',(0.,0.,1.));
#6394=DIRECTION('refdir',(1.,0.,0.));
#6395=DIRECTION('center_axis',(0.,1.,0.));
#6396=DIRECTION('ref_axis',(1.,0.,0.));
#6397=DIRECTION('center_axis',(0.,-1.,0.));
#6398=DIRECTION('ref_axis',(1.,0.,0.));
#6399=DIRECTION('',(0.,-1.,0.));
#6400=DIRECTION('center_axis',(0.,-1.,0.));
#6401=DIRECTION('ref_axis',(1.,0.,0.));
#6402=DIRECTION('center_axis',(0.,1.,0.));
#6403=DIRECTION('ref_axis',(1.,0.,0.));
#6404=DIRECTION('center_axis',(0.,1.,0.));
#6405=DIRECTION('ref_axis',(1.,0.,0.));
#6406=DIRECTION('',(0.,-1.,0.));
#6407=DIRECTION('center_axis',(0.,1.,0.));
#6408=DIRECTION('ref_axis',(1.,0.,0.));
#6409=DIRECTION('center_axis',(0.,1.,0.));
#6410=DIRECTION('ref_axis',(1.,0.,0.));
#6411=DIRECTION('center_axis',(0.,1.,0.));
#6412=DIRECTION('ref_axis',(1.,0.,0.));
#6413=DIRECTION('axis',(0.,0.,1.));
#6414=DIRECTION('refdir',(1.,0.,0.));
#6415=DIRECTION('center_axis',(0.,1.,0.));
#6416=DIRECTION('ref_axis',(1.,0.,0.));
#6417=DIRECTION('center_axis',(0.,-1.,0.));
#6418=DIRECTION('ref_axis',(1.,0.,0.));
#6419=DIRECTION('',(0.,-1.,0.));
#6420=DIRECTION('center_axis',(0.,-1.,0.));
#6421=DIRECTION('ref_axis',(1.,0.,0.));
#6422=DIRECTION('center_axis',(0.,1.,0.));
#6423=DIRECTION('ref_axis',(1.,0.,0.));
#6424=DIRECTION('center_axis',(0.,1.,0.));
#6425=DIRECTION('ref_axis',(1.,0.,0.));
#6426=DIRECTION('',(0.,-1.,0.));
#6427=DIRECTION('center_axis',(0.,1.,0.));
#6428=DIRECTION('ref_axis',(1.,0.,0.));
#6429=DIRECTION('center_axis',(0.,1.,0.));
#6430=DIRECTION('ref_axis',(1.,0.,0.));
#6431=DIRECTION('center_axis',(0.,1.,0.));
#6432=DIRECTION('ref_axis',(1.,0.,0.));
#6433=DIRECTION('axis',(0.,0.,1.));
#6434=DIRECTION('refdir',(1.,0.,0.));
#6435=DIRECTION('center_axis',(0.,0.,1.));
#6436=DIRECTION('ref_axis',(1.,0.,0.));
#6437=DIRECTION('center_axis',(0.,0.,-1.));
#6438=DIRECTION('ref_axis',(1.,0.,0.));
#6439=DIRECTION('',(0.,0.,-1.));
#6440=DIRECTION('center_axis',(0.,0.,-1.));
#6441=DIRECTION('ref_axis',(1.,0.,0.));
#6442=DIRECTION('center_axis',(0.,0.,1.));
#6443=DIRECTION('ref_axis',(1.,0.,0.));
#6444=DIRECTION('center_axis',(0.,0.,1.));
#6445=DIRECTION('ref_axis',(1.,0.,0.));
#6446=DIRECTION('',(0.,0.,-1.));
#6447=DIRECTION('center_axis',(0.,0.,1.));
#6448=DIRECTION('ref_axis',(1.,0.,0.));
#6449=DIRECTION('center_axis',(0.,0.,1.));
#6450=DIRECTION('ref_axis',(1.,0.,0.));
#6451=DIRECTION('center_axis',(0.,0.,1.));
#6452=DIRECTION('ref_axis',(1.,0.,0.));
#6453=DIRECTION('axis',(0.,0.,1.));
#6454=DIRECTION('refdir',(1.,0.,0.));
#6455=DIRECTION('center_axis',(0.,1.,0.));
#6456=DIRECTION('ref_axis',(1.,0.,0.));
#6457=DIRECTION('center_axis',(0.,-1.,0.));
#6458=DIRECTION('ref_axis',(1.,0.,0.));
#6459=DIRECTION('',(0.,-1.,0.));
#6460=DIRECTION('center_axis',(0.,-1.,0.));
#6461=DIRECTION('ref_axis',(1.,0.,0.));
#6462=DIRECTION('center_axis',(0.,1.,0.));
#6463=DIRECTION('ref_axis',(1.,0.,0.));
#6464=DIRECTION('center_axis',(0.,1.,0.));
#6465=DIRECTION('ref_axis',(1.,0.,0.));
#6466=DIRECTION('',(0.,-1.,0.));
#6467=DIRECTION('center_axis',(0.,1.,0.));
#6468=DIRECTION('ref_axis',(1.,0.,0.));
#6469=DIRECTION('center_axis',(0.,1.,0.));
#6470=DIRECTION('ref_axis',(1.,0.,0.));
#6471=DIRECTION('center_axis',(0.,1.,0.));
#6472=DIRECTION('ref_axis',(1.,0.,0.));
#6473=DIRECTION('axis',(0.,0.,1.));
#6474=DIRECTION('refdir',(1.,0.,0.));
#6475=DIRECTION('center_axis',(0.,1.,0.));
#6476=DIRECTION('ref_axis',(1.,0.,0.));
#6477=DIRECTION('center_axis',(0.,-1.,0.));
#6478=DIRECTION('ref_axis',(1.,0.,0.));
#6479=DIRECTION('',(0.,-1.,0.));
#6480=DIRECTION('center_axis',(0.,-1.,0.));
#6481=DIRECTION('ref_axis',(1.,0.,0.));
#6482=DIRECTION('center_axis',(0.,1.,0.));
#6483=DIRECTION('ref_axis',(1.,0.,0.));
#6484=DIRECTION('center_axis',(0.,1.,0.));
#6485=DIRECTION('ref_axis',(1.,0.,0.));
#6486=DIRECTION('',(0.,-1.,0.));
#6487=DIRECTION('center_axis',(0.,1.,0.));
#6488=DIRECTION('ref_axis',(1.,0.,0.));
#6489=DIRECTION('center_axis',(0.,1.,0.));
#6490=DIRECTION('ref_axis',(1.,0.,0.));
#6491=DIRECTION('center_axis',(0.,1.,0.));
#6492=DIRECTION('ref_axis',(1.,0.,0.));
#6493=DIRECTION('axis',(0.,0.,1.));
#6494=DIRECTION('refdir',(1.,0.,0.));
#6495=DIRECTION('center_axis',(0.866025403784439,0.,-0.5));
#6496=DIRECTION('ref_axis',(0.5,0.,0.866025403784439));
#6497=DIRECTION('',(-0.5,0.,-0.866025403784439));
#6498=DIRECTION('',(0.,-1.,0.));
#6499=DIRECTION('',(0.5,0.,0.866025403784439));
#6500=DIRECTION('',(0.,-1.,0.));
#6501=DIRECTION('center_axis',(1.60246890531964E-16,0.,-1.));
#6502=DIRECTION('ref_axis',(1.,0.,1.60246890531964E-16));
#6503=DIRECTION('',(-1.,0.,-1.60246890531964E-16));
#6504=DIRECTION('',(0.,-1.,0.));
#6505=DIRECTION('',(1.,0.,1.60246890531964E-16));
#6506=DIRECTION('center_axis',(-0.866025403784439,0.,-0.5));
#6507=DIRECTION('ref_axis',(0.5,0.,-0.866025403784439));
#6508=DIRECTION('',(-0.5,0.,0.866025403784439));
#6509=DIRECTION('',(0.,-1.,0.));
#6510=DIRECTION('',(0.5,0.,-0.866025403784439));
#6511=DIRECTION('center_axis',(-0.866025403784439,0.,0.5));
#6512=DIRECTION('ref_axis',(-0.5,0.,-0.866025403784439));
#6513=DIRECTION('',(0.5,0.,0.866025403784439));
#6514=DIRECTION('',(0.,-1.,0.));
#6515=DIRECTION('',(-0.5,0.,-0.866025403784439));
#6516=DIRECTION('center_axis',(-1.60246890531964E-16,0.,1.));
#6517=DIRECTION('ref_axis',(-1.,0.,-1.60246890531964E-16));
#6518=DIRECTION('',(1.,0.,1.60246890531964E-16));
#6519=DIRECTION('',(0.,-1.,0.));
#6520=DIRECTION('',(-1.,0.,-1.60246890531964E-16));
#6521=DIRECTION('center_axis',(0.866025403784439,0.,0.5));
#6522=DIRECTION('ref_axis',(-0.5,0.,0.866025403784439));
#6523=DIRECTION('',(0.5,0.,-0.866025403784439));
#6524=DIRECTION('',(-0.5,0.,0.866025403784439));
#6525=DIRECTION('center_axis',(0.,1.,0.));
#6526=DIRECTION('ref_axis',(1.,0.,0.));
#6527=DIRECTION('center_axis',(0.,-1.,0.));
#6528=DIRECTION('ref_axis',(0.,0.,-1.));
#6529=DIRECTION('center_axis',(0.,1.,0.));
#6530=DIRECTION('ref_axis',(1.,0.,0.));
#6531=DIRECTION('center_axis',(0.,1.,0.));
#6532=DIRECTION('ref_axis',(1.,0.,0.));
#6533=DIRECTION('center_axis',(0.,1.,0.));
#6534=DIRECTION('ref_axis',(1.,0.,0.));
#6535=DIRECTION('center_axis',(0.,1.,0.));
#6536=DIRECTION('ref_axis',(1.,0.,0.));
#6537=DIRECTION('',(0.,-1.,0.));
#6538=DIRECTION('center_axis',(0.,1.,0.));
#6539=DIRECTION('ref_axis',(1.,0.,0.));
#6540=DIRECTION('center_axis',(0.,1.,0.));
#6541=DIRECTION('ref_axis',(1.,0.,0.));
#6542=DIRECTION('center_axis',(0.,1.,0.));
#6543=DIRECTION('ref_axis',(0.,0.,1.));
#6544=DIRECTION('center_axis',(0.,-1.,0.));
#6545=DIRECTION('ref_axis',(1.,0.,0.));
#6546=DIRECTION('center_axis',(0.,-1.,0.));
#6547=DIRECTION('ref_axis',(1.,0.,0.));
#6548=DIRECTION('center_axis',(0.,-1.,0.));
#6549=DIRECTION('ref_axis',(1.,0.,0.));
#6550=DIRECTION('',(0.707106781186548,0.707106781186547,8.65956056235493E-17));
#6551=DIRECTION('center_axis',(0.,-1.,0.));
#6552=DIRECTION('ref_axis',(1.,0.,0.));
#6553=DIRECTION('center_axis',(0.,-1.,0.));
#6554=DIRECTION('ref_axis',(1.,0.,0.));
#6555=DIRECTION('',(0.,1.,0.));
#6556=DIRECTION('center_axis',(0.,1.,0.));
#6557=DIRECTION('ref_axis',(1.,0.,0.));
#6558=DIRECTION('center_axis',(0.,-1.,0.));
#6559=DIRECTION('ref_axis',(1.,0.,0.));
#6560=DIRECTION('',(-0.707106781186548,0.707106781186547,-8.65956056235494E-17));
#6561=DIRECTION('center_axis',(0.,-1.,0.));
#6562=DIRECTION('ref_axis',(0.,0.,-1.));
#6563=DIRECTION('center_axis',(0.,-1.,0.));
#6564=DIRECTION('ref_axis',(1.,0.,0.));
#6565=DIRECTION('center_axis',(0.,1.,0.));
#6566=DIRECTION('ref_axis',(1.,0.,0.));
#6567=DIRECTION('center_axis',(0.,1.,0.));
#6568=DIRECTION('ref_axis',(1.,0.,0.));
#6569=DIRECTION('',(-0.447213595499958,0.894427190999916,-5.47678698264203E-17));
#6570=DIRECTION('center_axis',(0.,-1.,0.));
#6571=DIRECTION('ref_axis',(1.,0.,0.));
#6572=DIRECTION('',(0.,1.,0.));
#6573=DIRECTION('axis',(0.,0.,1.));
#6574=DIRECTION('refdir',(1.,0.,0.));
#6575=DIRECTION('center_axis',(0.,1.,0.));
#6576=DIRECTION('ref_axis',(1.,0.,0.));
#6577=DIRECTION('center_axis',(0.,-1.,0.));
#6578=DIRECTION('ref_axis',(1.,0.,0.));
#6579=DIRECTION('',(0.,-1.,0.));
#6580=DIRECTION('center_axis',(0.,-1.,0.));
#6581=DIRECTION('ref_axis',(1.,0.,0.));
#6582=DIRECTION('center_axis',(0.,1.,0.));
#6583=DIRECTION('ref_axis',(1.,0.,0.));
#6584=DIRECTION('center_axis',(0.,1.,0.));
#6585=DIRECTION('ref_axis',(1.,0.,0.));
#6586=DIRECTION('',(0.,-1.,0.));
#6587=DIRECTION('center_axis',(0.,1.,0.));
#6588=DIRECTION('ref_axis',(1.,0.,0.));
#6589=DIRECTION('center_axis',(0.,1.,0.));
#6590=DIRECTION('ref_axis',(1.,0.,0.));
#6591=DIRECTION('center_axis',(0.,1.,0.));
#6592=DIRECTION('ref_axis',(1.,0.,0.));
#6593=DIRECTION('axis',(0.,0.,1.));
#6594=DIRECTION('refdir',(1.,0.,0.));
#6595=DIRECTION('center_axis',(0.,1.,0.));
#6596=DIRECTION('ref_axis',(1.,0.,0.));
#6597=DIRECTION('',(0.866025403784439,-0.5,1.06057523872491E-16));
#6598=DIRECTION('center_axis',(0.,-1.,0.));
#6599=DIRECTION('ref_axis',(1.,0.,0.));
#6600=DIRECTION('center_axis',(0.,-1.,0.));
#6601=DIRECTION('ref_axis',(1.,0.,0.));
#6602=DIRECTION('center_axis',(0.,1.,0.));
#6603=DIRECTION('ref_axis',(1.,0.,0.));
#6604=DIRECTION('',(-0.866025403784439,-0.5,-1.06057523872491E-16));
#6605=DIRECTION('center_axis',(1.4792020664489E-16,0.,-1.));
#6606=DIRECTION('ref_axis',(-1.,0.,-1.4792020664489E-16));
#6607=DIRECTION('',(0.,1.,0.));
#6608=DIRECTION('',(0.,1.,0.));
#6609=DIRECTION('center_axis',(-0.866025403784439,0.,-0.5));
#6610=DIRECTION('ref_axis',(-0.5,0.,0.866025403784439));
#6611=DIRECTION('',(0.,1.,0.));
#6612=DIRECTION('center_axis',(-0.866025403784439,0.,0.5));
#6613=DIRECTION('ref_axis',(0.5,0.,0.866025403784439));
#6614=DIRECTION('',(0.,1.,0.));
#6615=DIRECTION('center_axis',(0.,1.,0.));
#6616=DIRECTION('ref_axis',(1.,0.,0.));
#6617=DIRECTION('center_axis',(0.,1.,0.));
#6618=DIRECTION('ref_axis',(1.,0.,0.));
#6619=DIRECTION('',(0.,-1.,0.));
#6620=DIRECTION('center_axis',(0.,1.,0.));
#6621=DIRECTION('ref_axis',(1.,0.,0.));
#6622=DIRECTION('center_axis',(-2.95840413289779E-16,0.,1.));
#6623=DIRECTION('ref_axis',(1.,0.,2.95840413289779E-16));
#6624=DIRECTION('',(0.,1.,0.));
#6625=DIRECTION('center_axis',(0.866025403784439,0.,-0.5));
#6626=DIRECTION('ref_axis',(-0.5,0.,-0.866025403784439));
#6627=DIRECTION('',(0.,1.,0.));
#6628=DIRECTION('center_axis',(0.866025403784439,0.,0.5));
#6629=DIRECTION('ref_axis',(0.5,0.,-0.866025403784439));
#6630=DIRECTION('center_axis',(0.,1.,0.));
#6631=DIRECTION('ref_axis',(1.,0.,0.));
#6632=DIRECTION('center_axis',(0.,1.,0.));
#6633=DIRECTION('ref_axis',(1.,0.,0.));
#6634=DIRECTION('axis',(0.,0.,1.));
#6635=DIRECTION('refdir',(1.,0.,0.));
#6636=DIRECTION('center_axis',(0.,1.,0.));
#6637=DIRECTION('ref_axis',(0.,0.,1.));
#6638=DIRECTION('center_axis',(0.,-1.,0.));
#6639=DIRECTION('ref_axis',(1.,0.,0.));
#6640=DIRECTION('center_axis',(0.,-1.,0.));
#6641=DIRECTION('ref_axis',(1.,0.,0.));
#6642=DIRECTION('center_axis',(0.,-1.,0.));
#6643=DIRECTION('ref_axis',(1.,0.,0.));
#6644=DIRECTION('',(0.707106781186548,0.707106781186547,8.65956056235493E-17));
#6645=DIRECTION('center_axis',(0.,-1.,0.));
#6646=DIRECTION('ref_axis',(1.,0.,0.));
#6647=DIRECTION('center_axis',(0.,-1.,0.));
#6648=DIRECTION('ref_axis',(1.,0.,0.));
#6649=DIRECTION('',(0.,1.,0.));
#6650=DIRECTION('center_axis',(0.,1.,0.));
#6651=DIRECTION('ref_axis',(1.,0.,0.));
#6652=DIRECTION('center_axis',(0.,-1.,0.));
#6653=DIRECTION('ref_axis',(1.,0.,0.));
#6654=DIRECTION('',(-0.707106781186548,0.707106781186547,-8.65956056235494E-17));
#6655=DIRECTION('center_axis',(0.,-1.,0.));
#6656=DIRECTION('ref_axis',(0.,0.,-1.));
#6657=DIRECTION('center_axis',(0.,-1.,0.));
#6658=DIRECTION('ref_axis',(1.,0.,0.));
#6659=DIRECTION('center_axis',(0.,1.,0.));
#6660=DIRECTION('ref_axis',(1.,0.,0.));
#6661=DIRECTION('center_axis',(0.,1.,0.));
#6662=DIRECTION('ref_axis',(1.,0.,0.));
#6663=DIRECTION('',(-0.447213595499958,0.894427190999916,-5.47678698264203E-17));
#6664=DIRECTION('center_axis',(0.,-1.,0.));
#6665=DIRECTION('ref_axis',(1.,0.,0.));
#6666=DIRECTION('center_axis',(0.,1.,0.));
#6667=DIRECTION('ref_axis',(1.,0.,0.));
#6668=DIRECTION('',(0.,1.,0.));
#6669=DIRECTION('center_axis',(0.,1.,0.));
#6670=DIRECTION('ref_axis',(1.,0.,0.));
#6671=DIRECTION('center_axis',(0.,-1.,0.));
#6672=DIRECTION('ref_axis',(1.,0.,0.));
#6673=DIRECTION('',(-0.707106781186547,0.707106781186548,-8.65956056235493E-17));
#6674=DIRECTION('center_axis',(0.,-1.,0.));
#6675=DIRECTION('ref_axis',(0.,0.,-1.));
#6676=DIRECTION('center_axis',(0.866025403784439,0.,-0.5));
#6677=DIRECTION('ref_axis',(0.5,0.,0.866025403784439));
#6678=DIRECTION('',(-0.5,0.,-0.866025403784439));
#6679=DIRECTION('',(0.,-1.,0.));
#6680=DIRECTION('',(0.5,0.,0.866025403784439));
#6681=DIRECTION('',(0.,-1.,0.));
#6682=DIRECTION('center_axis',(1.60246890531964E-16,0.,-1.));
#6683=DIRECTION('ref_axis',(1.,0.,1.60246890531964E-16));
#6684=DIRECTION('',(-1.,0.,-1.60246890531964E-16));
#6685=DIRECTION('',(0.,-1.,0.));
#6686=DIRECTION('',(1.,0.,1.60246890531964E-16));
#6687=DIRECTION('center_axis',(-0.866025403784439,0.,-0.5));
#6688=DIRECTION('ref_axis',(0.5,0.,-0.866025403784439));
#6689=DIRECTION('',(-0.5,0.,0.866025403784439));
#6690=DIRECTION('',(0.,-1.,0.));
#6691=DIRECTION('',(0.5,0.,-0.866025403784439));
#6692=DIRECTION('center_axis',(-0.866025403784439,0.,0.5));
#6693=DIRECTION('ref_axis',(-0.5,0.,-0.866025403784439));
#6694=DIRECTION('',(0.5,0.,0.866025403784439));
#6695=DIRECTION('',(0.,-1.,0.));
#6696=DIRECTION('',(-0.5,0.,-0.866025403784439));
#6697=DIRECTION('center_axis',(-1.60246890531964E-16,0.,1.));
#6698=DIRECTION('ref_axis',(-1.,0.,-1.60246890531964E-16));
#6699=DIRECTION('',(1.,0.,1.60246890531964E-16));
#6700=DIRECTION('',(0.,-1.,0.));
#6701=DIRECTION('',(-1.,0.,-1.60246890531964E-16));
#6702=DIRECTION('center_axis',(0.866025403784439,0.,0.5));
#6703=DIRECTION('ref_axis',(-0.5,0.,0.866025403784439));
#6704=DIRECTION('',(0.5,0.,-0.866025403784439));
#6705=DIRECTION('',(-0.5,0.,0.866025403784439));
#6706=DIRECTION('center_axis',(0.,1.,0.));
#6707=DIRECTION('ref_axis',(1.,0.,0.));
#6708=DIRECTION('center_axis',(0.,-1.,0.));
#6709=DIRECTION('ref_axis',(0.,0.,-1.));
#6710=DIRECTION('',(0.,0.,1.));
#6711=DIRECTION('',(1.,0.,0.));
#6712=DIRECTION('',(0.,0.,1.));
#6713=DIRECTION('',(1.,0.,0.));
#6714=DIRECTION('',(0.,0.,1.));
#6715=DIRECTION('',(1.,0.,0.));
#6716=DIRECTION('',(0.,0.,1.));
#6717=DIRECTION('',(1.,0.,0.));
#6718=DIRECTION('',(0.,0.,1.));
#6719=DIRECTION('',(1.,0.,0.));
#6720=DIRECTION('',(0.,0.,1.));
#6721=DIRECTION('',(1.,0.,0.));
#6722=DIRECTION('',(0.,0.,1.));
#6723=DIRECTION('',(1.,0.,0.));
#6724=DIRECTION('',(0.,0.,1.));
#6725=DIRECTION('',(1.,0.,0.));
#6726=DIRECTION('',(0.,0.,1.));
#6727=DIRECTION('',(1.,0.,0.));
#6728=DIRECTION('',(0.,0.,1.));
#6729=DIRECTION('',(1.,0.,0.));
#6730=DIRECTION('',(0.,0.,1.));
#6731=DIRECTION('',(1.,0.,0.));
#6732=DIRECTION('',(0.,0.,1.));
#6733=DIRECTION('',(1.,0.,0.));
#6734=DIRECTION('',(0.,0.,1.));
#6735=DIRECTION('',(1.,0.,0.));
#6736=DIRECTION('',(0.,0.,1.));
#6737=DIRECTION('',(1.,0.,0.));
#6738=DIRECTION('',(0.,0.,1.));
#6739=DIRECTION('',(1.,0.,0.));
#6740=DIRECTION('',(0.,0.,1.));
#6741=DIRECTION('',(1.,0.,0.));
#6742=DIRECTION('',(0.,0.,1.));
#6743=DIRECTION('',(1.,0.,0.));
#6744=DIRECTION('',(0.,0.,1.));
#6745=DIRECTION('',(1.,0.,0.));
#6746=DIRECTION('',(0.,0.,1.));
#6747=DIRECTION('',(1.,0.,0.));
#6748=DIRECTION('',(0.,0.,1.));
#6749=DIRECTION('',(1.,0.,0.));
#6750=DIRECTION('',(0.,0.,1.));
#6751=DIRECTION('',(1.,0.,0.));
#6752=DIRECTION('',(0.,0.,1.));
#6753=DIRECTION('',(1.,0.,0.));
#6754=DIRECTION('',(0.,0.,1.));
#6755=DIRECTION('',(1.,0.,0.));
#6756=DIRECTION('',(0.,0.,1.));
#6757=DIRECTION('',(1.,0.,0.));
#6758=DIRECTION('',(0.,0.,1.));
#6759=DIRECTION('',(1.,0.,0.));
#6760=DIRECTION('axis',(0.,0.,1.));
#6761=DIRECTION('refdir',(1.,0.,0.));
#6762=DIRECTION('axis',(0.,0.,1.));
#6763=DIRECTION('refdir',(1.,0.,0.));
#6764=DIRECTION('center_axis',(0.,1.,0.));
#6765=DIRECTION('ref_axis',(1.,0.,0.));
#6766=DIRECTION('center_axis',(0.,1.,0.));
#6767=DIRECTION('ref_axis',(1.,0.,0.));
#6768=DIRECTION('',(0.,1.,0.));
#6769=DIRECTION('center_axis',(0.,-1.,0.));
#6770=DIRECTION('ref_axis',(1.,0.,0.));
#6771=DIRECTION('center_axis',(0.,1.,0.));
#6772=DIRECTION('ref_axis',(1.,0.,0.));
#6773=DIRECTION('center_axis',(0.,1.,0.));
#6774=DIRECTION('ref_axis',(1.,0.,0.));
#6775=DIRECTION('',(0.,1.,0.));
#6776=DIRECTION('center_axis',(0.,-1.,0.));
#6777=DIRECTION('ref_axis',(1.,0.,0.));
#6778=DIRECTION('center_axis',(0.,1.,0.));
#6779=DIRECTION('ref_axis',(1.,0.,0.));
#6780=DIRECTION('center_axis',(0.,1.,0.));
#6781=DIRECTION('ref_axis',(1.,0.,0.));
#6782=DIRECTION('',(0.,1.,0.));
#6783=DIRECTION('center_axis',(0.,-1.,0.));
#6784=DIRECTION('ref_axis',(1.,0.,0.));
#6785=DIRECTION('center_axis',(0.,1.,0.));
#6786=DIRECTION('ref_axis',(1.,0.,0.));
#6787=DIRECTION('center_axis',(0.,1.,0.));
#6788=DIRECTION('ref_axis',(1.,0.,0.));
#6789=DIRECTION('',(0.,1.,0.));
#6790=DIRECTION('center_axis',(0.,-1.,0.));
#6791=DIRECTION('ref_axis',(1.,0.,0.));
#6792=DIRECTION('center_axis',(0.,-1.,0.));
#6793=DIRECTION('ref_axis',(1.,0.,0.));
#6794=DIRECTION('center_axis',(0.,-1.,0.));
#6795=DIRECTION('ref_axis',(1.,0.,0.));
#6796=DIRECTION('',(-0.707106781186547,-0.707106781186548,-8.65956056235493E-17));
#6797=DIRECTION('center_axis',(0.,-1.,0.));
#6798=DIRECTION('ref_axis',(1.,0.,0.));
#6799=DIRECTION('center_axis',(0.,1.,0.));
#6800=DIRECTION('ref_axis',(1.,0.,0.));
#6801=DIRECTION('center_axis',(0.,1.,0.));
#6802=DIRECTION('ref_axis',(1.,0.,0.));
#6803=DIRECTION('',(0.707106781186547,-0.707106781186548,8.65956056235493E-17));
#6804=DIRECTION('center_axis',(0.,1.,0.));
#6805=DIRECTION('ref_axis',(1.,0.,0.));
#6806=DIRECTION('center_axis',(0.,1.,0.));
#6807=DIRECTION('ref_axis',(1.,0.,0.));
#6808=DIRECTION('',(0.,-1.,0.));
#6809=DIRECTION('center_axis',(0.,1.,0.));
#6810=DIRECTION('ref_axis',(1.,0.,0.));
#6811=DIRECTION('center_axis',(0.,1.,0.));
#6812=DIRECTION('ref_axis',(1.,0.,0.));
#6813=DIRECTION('center_axis',(0.,1.,0.));
#6814=DIRECTION('ref_axis',(1.,0.,0.));
#6815=DIRECTION('center_axis',(0.,1.,0.));
#6816=DIRECTION('ref_axis',(1.,0.,0.));
#6817=DIRECTION('center_axis',(0.,-1.,0.));
#6818=DIRECTION('ref_axis',(1.,0.,0.));
#6819=DIRECTION('center_axis',(0.,1.,0.));
#6820=DIRECTION('ref_axis',(1.,0.,0.));
#6821=DIRECTION('',(0.,-1.,0.));
#6822=DIRECTION('center_axis',(0.,1.,0.));
#6823=DIRECTION('ref_axis',(1.,0.,0.));
#6824=DIRECTION('',(0.,-1.,0.));
#6825=DIRECTION('center_axis',(0.,1.,0.));
#6826=DIRECTION('ref_axis',(1.,0.,0.));
#6827=DIRECTION('center_axis',(0.,1.,0.));
#6828=DIRECTION('ref_axis',(1.,0.,0.));
#6829=DIRECTION('center_axis',(0.,-1.,0.));
#6830=DIRECTION('ref_axis',(1.,0.,0.));
#6831=DIRECTION('',(0.,-1.,0.));
#6832=DIRECTION('center_axis',(0.,-1.,0.));
#6833=DIRECTION('ref_axis',(1.,0.,0.));
#6834=DIRECTION('center_axis',(0.,1.,0.));
#6835=DIRECTION('ref_axis',(1.,0.,0.));
#6836=DIRECTION('center_axis',(0.,1.,0.));
#6837=DIRECTION('ref_axis',(1.,0.,0.));
#6838=DIRECTION('',(0.,-1.,0.));
#6839=DIRECTION('center_axis',(0.,1.,0.));
#6840=DIRECTION('ref_axis',(1.,0.,0.));
#6841=DIRECTION('center_axis',(0.,1.,0.));
#6842=DIRECTION('ref_axis',(1.,0.,0.));
#6843=DIRECTION('axis',(0.,0.,1.));
#6844=DIRECTION('refdir',(1.,0.,0.));
#6845=DIRECTION('center_axis',(0.,1.,0.));
#6846=DIRECTION('ref_axis',(1.,0.,0.));
#6847=DIRECTION('center_axis',(0.,-1.,0.));
#6848=DIRECTION('ref_axis',(1.,0.,0.));
#6849=DIRECTION('',(0.,-1.,0.));
#6850=DIRECTION('center_axis',(0.,-1.,0.));
#6851=DIRECTION('ref_axis',(1.,0.,0.));
#6852=DIRECTION('center_axis',(0.,1.,0.));
#6853=DIRECTION('ref_axis',(1.,0.,0.));
#6854=DIRECTION('center_axis',(0.,1.,0.));
#6855=DIRECTION('ref_axis',(1.,0.,0.));
#6856=DIRECTION('',(0.,-1.,0.));
#6857=DIRECTION('center_axis',(0.,1.,0.));
#6858=DIRECTION('ref_axis',(1.,0.,0.));
#6859=DIRECTION('center_axis',(0.,1.,0.));
#6860=DIRECTION('ref_axis',(1.,0.,0.));
#6861=DIRECTION('center_axis',(0.,1.,0.));
#6862=DIRECTION('ref_axis',(1.,0.,0.));
#6863=DIRECTION('axis',(0.,0.,1.));
#6864=DIRECTION('refdir',(1.,0.,0.));
#6865=DIRECTION('center_axis',(0.,1.,0.));
#6866=DIRECTION('ref_axis',(1.,0.,0.));
#6867=DIRECTION('center_axis',(0.,1.,0.));
#6868=DIRECTION('ref_axis',(1.,0.,0.));
#6869=DIRECTION('',(0.,1.,0.));
#6870=DIRECTION('center_axis',(0.,-1.,0.));
#6871=DIRECTION('ref_axis',(1.,0.,0.));
#6872=DIRECTION('center_axis',(0.,1.,0.));
#6873=DIRECTION('ref_axis',(1.,0.,0.));
#6874=DIRECTION('center_axis',(0.,1.,0.));
#6875=DIRECTION('ref_axis',(1.,0.,0.));
#6876=DIRECTION('',(0.,1.,0.));
#6877=DIRECTION('center_axis',(0.,-1.,0.));
#6878=DIRECTION('ref_axis',(1.,0.,0.));
#6879=DIRECTION('center_axis',(0.,1.,0.));
#6880=DIRECTION('ref_axis',(1.,0.,0.));
#6881=DIRECTION('center_axis',(0.,1.,0.));
#6882=DIRECTION('ref_axis',(1.,0.,0.));
#6883=DIRECTION('',(0.,1.,0.));
#6884=DIRECTION('center_axis',(0.,-1.,0.));
#6885=DIRECTION('ref_axis',(1.,0.,0.));
#6886=DIRECTION('center_axis',(0.,1.,0.));
#6887=DIRECTION('ref_axis',(1.,0.,0.));
#6888=DIRECTION('center_axis',(0.,1.,0.));
#6889=DIRECTION('ref_axis',(1.,0.,0.));
#6890=DIRECTION('',(0.,1.,0.));
#6891=DIRECTION('center_axis',(0.,-1.,0.));
#6892=DIRECTION('ref_axis',(1.,0.,0.));
#6893=DIRECTION('center_axis',(0.,1.,0.));
#6894=DIRECTION('ref_axis',(1.,0.,0.));
#6895=DIRECTION('center_axis',(0.,1.,0.));
#6896=DIRECTION('ref_axis',(1.,0.,0.));
#6897=DIRECTION('',(0.,-1.,0.));
#6898=DIRECTION('center_axis',(0.,-1.,0.));
#6899=DIRECTION('ref_axis',(1.,0.,0.));
#6900=DIRECTION('center_axis',(0.,1.,0.));
#6901=DIRECTION('ref_axis',(1.,0.,0.));
#6902=DIRECTION('center_axis',(0.,-1.,0.));
#6903=DIRECTION('ref_axis',(1.,0.,0.));
#6904=DIRECTION('center_axis',(0.,1.,0.));
#6905=DIRECTION('ref_axis',(1.,0.,0.));
#6906=DIRECTION('',(0.,-1.,0.));
#6907=DIRECTION('center_axis',(0.,-1.,0.));
#6908=DIRECTION('ref_axis',(1.,0.,0.));
#6909=DIRECTION('center_axis',(0.,1.,0.));
#6910=DIRECTION('ref_axis',(1.,0.,0.));
#6911=DIRECTION('center_axis',(0.,1.,0.));
#6912=DIRECTION('ref_axis',(1.,0.,0.));
#6913=DIRECTION('',(0.,-1.,0.));
#6914=DIRECTION('center_axis',(0.,1.,0.));
#6915=DIRECTION('ref_axis',(1.,0.,0.));
#6916=DIRECTION('center_axis',(0.,1.,0.));
#6917=DIRECTION('ref_axis',(1.,0.,0.));
#6918=DIRECTION('center_axis',(0.,1.,0.));
#6919=DIRECTION('ref_axis',(1.,0.,0.));
#6920=DIRECTION('axis',(0.,0.,1.));
#6921=DIRECTION('refdir',(1.,0.,0.));
#6922=DIRECTION('center_axis',(0.,1.,0.));
#6923=DIRECTION('ref_axis',(1.,0.,0.));
#6924=DIRECTION('center_axis',(0.,1.,0.));
#6925=DIRECTION('ref_axis',(1.,0.,0.));
#6926=DIRECTION('',(0.,1.,0.));
#6927=DIRECTION('center_axis',(0.,-1.,0.));
#6928=DIRECTION('ref_axis',(1.,0.,0.));
#6929=DIRECTION('center_axis',(0.,1.,0.));
#6930=DIRECTION('ref_axis',(1.,0.,0.));
#6931=DIRECTION('center_axis',(0.,1.,0.));
#6932=DIRECTION('ref_axis',(1.,0.,0.));
#6933=DIRECTION('',(0.,1.,0.));
#6934=DIRECTION('center_axis',(0.,-1.,0.));
#6935=DIRECTION('ref_axis',(1.,0.,0.));
#6936=DIRECTION('center_axis',(0.,1.,0.));
#6937=DIRECTION('ref_axis',(1.,0.,0.));
#6938=DIRECTION('center_axis',(0.,1.,0.));
#6939=DIRECTION('ref_axis',(1.,0.,0.));
#6940=DIRECTION('',(0.,1.,0.));
#6941=DIRECTION('center_axis',(0.,-1.,0.));
#6942=DIRECTION('ref_axis',(1.,0.,0.));
#6943=DIRECTION('center_axis',(0.,1.,0.));
#6944=DIRECTION('ref_axis',(1.,0.,0.));
#6945=DIRECTION('center_axis',(0.,1.,0.));
#6946=DIRECTION('ref_axis',(1.,0.,0.));
#6947=DIRECTION('',(0.,1.,0.));
#6948=DIRECTION('center_axis',(0.,-1.,0.));
#6949=DIRECTION('ref_axis',(1.,0.,0.));
#6950=DIRECTION('center_axis',(0.,1.,0.));
#6951=DIRECTION('ref_axis',(1.,0.,0.));
#6952=DIRECTION('center_axis',(0.,1.,0.));
#6953=DIRECTION('ref_axis',(1.,0.,0.));
#6954=DIRECTION('',(0.,-1.,0.));
#6955=DIRECTION('center_axis',(0.,1.,0.));
#6956=DIRECTION('ref_axis',(1.,0.,0.));
#6957=DIRECTION('center_axis',(0.,1.,0.));
#6958=DIRECTION('ref_axis',(1.,0.,0.));
#6959=DIRECTION('center_axis',(0.,-1.,0.));
#6960=DIRECTION('ref_axis',(1.,0.,0.));
#6961=DIRECTION('center_axis',(0.,1.,0.));
#6962=DIRECTION('ref_axis',(1.,0.,0.));
#6963=DIRECTION('center_axis',(0.,-1.,0.));
#6964=DIRECTION('ref_axis',(1.,0.,0.));
#6965=DIRECTION('',(0.,-1.,0.));
#6966=DIRECTION('center_axis',(0.,1.,0.));
#6967=DIRECTION('ref_axis',(1.,0.,0.));
#6968=DIRECTION('center_axis',(0.,1.,0.));
#6969=DIRECTION('ref_axis',(1.,0.,0.));
#6970=DIRECTION('',(0.,-1.,0.));
#6971=DIRECTION('center_axis',(0.,1.,0.));
#6972=DIRECTION('ref_axis',(1.,0.,0.));
#6973=DIRECTION('center_axis',(0.,1.,0.));
#6974=DIRECTION('ref_axis',(1.,0.,0.));
#6975=DIRECTION('center_axis',(0.,1.,0.));
#6976=DIRECTION('ref_axis',(1.,0.,0.));
#6977=DIRECTION('axis',(0.,0.,1.));
#6978=DIRECTION('refdir',(1.,0.,0.));
#6979=DIRECTION('axis',(0.,0.,1.));
#6980=DIRECTION('refdir',(1.,0.,0.));
#6981=DIRECTION('center_axis',(0.,-1.,0.));
#6982=DIRECTION('ref_axis',(0.,0.,-1.));
#6983=DIRECTION('center_axis',(0.,-1.,0.));
#6984=DIRECTION('ref_axis',(1.,0.,0.));
#6985=DIRECTION('center_axis',(0.,-1.,0.));
#6986=DIRECTION('ref_axis',(1.,0.,0.));
#6987=DIRECTION('center_axis',(1.,0.,1.22464679914735E-16));
#6988=DIRECTION('ref_axis',(-1.22464679914735E-16,0.,1.));
#6989=DIRECTION('center_axis',(0.,1.,0.));
#6990=DIRECTION('ref_axis',(1.,0.,0.));
#6991=DIRECTION('center_axis',(0.,1.,0.));
#6992=DIRECTION('ref_axis',(1.,0.,0.));
#6993=DIRECTION('center_axis',(0.,-1.,0.));
#6994=DIRECTION('ref_axis',(1.,0.,0.));
#6995=DIRECTION('',(0.,1.,0.));
#6996=DIRECTION('center_axis',(0.,-1.,0.));
#6997=DIRECTION('ref_axis',(1.,0.,0.));
#6998=DIRECTION('center_axis',(0.,-1.,0.));
#6999=DIRECTION('ref_axis',(1.,0.,0.));
#7000=DIRECTION('center_axis',(0.,-1.,0.));
#7001=DIRECTION('ref_axis',(1.,0.,0.));
#7002=DIRECTION('',(0.,1.,0.));
#7003=DIRECTION('center_axis',(0.,-1.,0.));
#7004=DIRECTION('ref_axis',(1.,0.,0.));
#7005=DIRECTION('center_axis',(0.,1.,0.));
#7006=DIRECTION('ref_axis',(1.,0.,0.));
#7007=DIRECTION('',(-0.707106781186548,0.707106781186547,-8.65956056235494E-17));
#7008=DIRECTION('center_axis',(0.,-1.,0.));
#7009=DIRECTION('ref_axis',(1.,0.,0.));
#7010=DIRECTION('center_axis',(0.,1.,0.));
#7011=DIRECTION('ref_axis',(0.,0.,1.));
#7012=DIRECTION('center_axis',(0.,-1.,0.));
#7013=DIRECTION('ref_axis',(1.,0.,0.));
#7014=DIRECTION('center_axis',(0.,-1.,0.));
#7015=DIRECTION('ref_axis',(1.,0.,0.));
#7016=DIRECTION('',(0.,1.,0.));
#7017=DIRECTION('center_axis',(0.,-1.,0.));
#7018=DIRECTION('ref_axis',(0.,0.,-1.));
#7019=DIRECTION('center_axis',(0.,-1.,0.));
#7020=DIRECTION('ref_axis',(1.,0.,0.));
#7021=DIRECTION('center_axis',(0.,-1.,0.));
#7022=DIRECTION('ref_axis',(1.,0.,0.));
#7023=DIRECTION('',(0.707106781186548,0.707106781186547,8.65956056235494E-17));
#7024=DIRECTION('axis',(0.,0.,1.));
#7025=DIRECTION('refdir',(1.,0.,0.));
#7026=DIRECTION('center_axis',(0.,-1.,0.));
#7027=DIRECTION('ref_axis',(0.,0.,-1.));
#7028=DIRECTION('center_axis',(0.,-1.,0.));
#7029=DIRECTION('ref_axis',(1.,0.,0.));
#7030=DIRECTION('center_axis',(0.,-1.,0.));
#7031=DIRECTION('ref_axis',(1.,0.,0.));
#7032=DIRECTION('center_axis',(1.,0.,1.22464679914735E-16));
#7033=DIRECTION('ref_axis',(-1.22464679914735E-16,0.,1.));
#7034=DIRECTION('center_axis',(0.,1.,0.));
#7035=DIRECTION('ref_axis',(1.,0.,0.));
#7036=DIRECTION('center_axis',(0.,1.,0.));
#7037=DIRECTION('ref_axis',(1.,0.,0.));
#7038=DIRECTION('center_axis',(0.,-1.,0.));
#7039=DIRECTION('ref_axis',(1.,0.,0.));
#7040=DIRECTION('center_axis',(0.,-1.,0.));
#7041=DIRECTION('ref_axis',(1.,0.,0.));
#7042=DIRECTION('',(0.,1.,0.));
#7043=DIRECTION('center_axis',(0.,1.,0.));
#7044=DIRECTION('ref_axis',(0.,0.,1.));
#7045=DIRECTION('center_axis',(0.,-1.,0.));
#7046=DIRECTION('ref_axis',(1.,0.,0.));
#7047=DIRECTION('center_axis',(0.,-1.,0.));
#7048=DIRECTION('ref_axis',(1.,0.,0.));
#7049=DIRECTION('center_axis',(0.,-1.,0.));
#7050=DIRECTION('ref_axis',(1.,0.,0.));
#7051=DIRECTION('center_axis',(0.,-1.,0.));
#7052=DIRECTION('ref_axis',(1.,0.,0.));
#7053=DIRECTION('',(0.707106781186548,0.707106781186547,8.65956056235494E-17));
#7054=DIRECTION('center_axis',(0.,-1.,0.));
#7055=DIRECTION('ref_axis',(1.,0.,0.));
#7056=DIRECTION('center_axis',(0.,-1.,0.));
#7057=DIRECTION('ref_axis',(1.,0.,0.));
#7058=DIRECTION('',(0.,1.,0.));
#7059=DIRECTION('center_axis',(0.,1.,0.));
#7060=DIRECTION('ref_axis',(1.,0.,0.));
#7061=DIRECTION('center_axis',(0.,-1.,0.));
#7062=DIRECTION('ref_axis',(1.,0.,0.));
#7063=DIRECTION('',(-0.707106781186548,0.707106781186547,-8.65956056235494E-17));
#7064=DIRECTION('center_axis',(0.,-1.,0.));
#7065=DIRECTION('ref_axis',(0.,0.,-1.));
#7066=DIRECTION('center_axis',(0.,-1.,0.));
#7067=DIRECTION('ref_axis',(1.,0.,0.));
#7068=DIRECTION('',(0.,1.,0.));
#7069=DIRECTION('axis',(0.,0.,1.));
#7070=DIRECTION('refdir',(1.,0.,0.));
#7071=DIRECTION('center_axis',(0.,0.,1.));
#7072=DIRECTION('ref_axis',(1.,0.,0.));
#7073=DIRECTION('center_axis',(1.22464679914735E-16,-1.,0.));
#7074=DIRECTION('ref_axis',(-1.,-1.22464679914735E-16,0.));
#7075=DIRECTION('center_axis',(0.707106781186548,0.,0.707106781186548));
#7076=DIRECTION('ref_axis',(0.707106781186548,0.,-0.707106781186548));
#7077=DIRECTION('center_axis',(8.65956056235493E-17,-1.,-8.65956056235493E-17));
#7078=DIRECTION('ref_axis',(-0.707106781186548,-1.22464679914735E-16,0.707106781186548));
#7079=DIRECTION('center_axis',(1.,0.,0.));
#7080=DIRECTION('ref_axis',(6.12323399573677E-17,0.,-1.));
#7081=DIRECTION('center_axis',(7.49879891330929E-33,-1.,-1.22464679914735E-16));
#7082=DIRECTION('ref_axis',(-6.12323399573677E-17,-1.22464679914735E-16,
1.));
#7083=DIRECTION('center_axis',(0.707106781186548,0.,-0.707106781186548));
#7084=DIRECTION('ref_axis',(-0.707106781186548,0.,-0.707106781186548));
#7085=DIRECTION('center_axis',(-8.65956056235493E-17,-1.,-8.65956056235493E-17));
#7086=DIRECTION('ref_axis',(0.707106781186548,-1.22464679914735E-16,0.707106781186548));
#7087=DIRECTION('center_axis',(0.,0.,-1.));
#7088=DIRECTION('ref_axis',(-1.,0.,-1.22464679914735E-16));
#7089=DIRECTION('center_axis',(-1.22464679914735E-16,-1.,-1.49975978266186E-32));
#7090=DIRECTION('ref_axis',(1.,-1.22464679914735E-16,1.22464679914735E-16));
#7091=DIRECTION('center_axis',(-0.707106781186548,0.,-0.707106781186548));
#7092=DIRECTION('ref_axis',(-0.707106781186548,0.,0.707106781186548));
#7093=DIRECTION('center_axis',(-8.65956056235493E-17,-1.,8.65956056235493E-17));
#7094=DIRECTION('ref_axis',(0.707106781186548,-1.22464679914735E-16,-0.707106781186548));
#7095=DIRECTION('center_axis',(-1.,0.,0.));
#7096=DIRECTION('ref_axis',(-1.83697019872103E-16,0.,1.));
#7097=DIRECTION('center_axis',(-2.24963967399279E-32,-1.,1.22464679914735E-16));
#7098=DIRECTION('ref_axis',(1.83697019872103E-16,-1.22464679914735E-16,
-1.));
#7099=DIRECTION('center_axis',(-0.707106781186548,0.,0.707106781186548));
#7100=DIRECTION('ref_axis',(0.707106781186548,0.,0.707106781186548));
#7101=DIRECTION('center_axis',(8.65956056235493E-17,-1.,8.65956056235494E-17));
#7102=DIRECTION('ref_axis',(-0.707106781186548,-1.22464679914735E-16,-0.707106781186548));
#7103=DIRECTION('axis',(0.,0.,1.));
#7104=DIRECTION('refdir',(1.,0.,0.));
#7105=DIRECTION('center_axis',(0.,0.,1.));
#7106=DIRECTION('ref_axis',(1.,0.,0.));
#7107=DIRECTION('center_axis',(0.,-1.,0.));
#7108=DIRECTION('ref_axis',(0.,0.,-1.));
#7109=DIRECTION('center_axis',(0.,-1.,0.));
#7110=DIRECTION('ref_axis',(0.,0.,-1.));
#7111=DIRECTION('center_axis',(0.,1.,0.));
#7112=DIRECTION('ref_axis',(1.,0.,0.));
#7113=DIRECTION('center_axis',(0.,1.,0.));
#7114=DIRECTION('ref_axis',(1.,0.,0.));
#7115=DIRECTION('center_axis',(0.,1.,0.));
#7116=DIRECTION('ref_axis',(1.,0.,0.));
#7117=DIRECTION('center_axis',(0.,1.,0.));
#7118=DIRECTION('ref_axis',(1.,0.,0.));
#7119=DIRECTION('',(0.,-1.,0.));
#7120=DIRECTION('center_axis',(0.,-1.,0.));
#7121=DIRECTION('ref_axis',(1.,0.,0.));
#7122=DIRECTION('center_axis',(0.,1.,0.));
#7123=DIRECTION('ref_axis',(1.,0.,0.));
#7124=DIRECTION('center_axis',(0.,1.,0.));
#7125=DIRECTION('ref_axis',(1.,0.,0.));
#7126=DIRECTION('center_axis',(0.,1.,0.));
#7127=DIRECTION('ref_axis',(1.,0.,0.));
#7128=DIRECTION('center_axis',(0.,1.,0.));
#7129=DIRECTION('ref_axis',(1.,0.,0.));
#7130=DIRECTION('center_axis',(0.,1.,0.));
#7131=DIRECTION('ref_axis',(1.,0.,0.));
#7132=DIRECTION('center_axis',(0.,1.,0.));
#7133=DIRECTION('ref_axis',(1.,0.,0.));
#7134=DIRECTION('center_axis',(0.,-1.,0.));
#7135=DIRECTION('ref_axis',(1.,0.,0.));
#7136=DIRECTION('center_axis',(0.,-1.,0.));
#7137=DIRECTION('ref_axis',(0.,0.,-1.));
#7138=DIRECTION('center_axis',(6.12323399573677E-17,0.,1.));
#7139=DIRECTION('ref_axis',(1.,0.,0.));
#7140=DIRECTION('center_axis',(0.,-1.,0.));
#7141=DIRECTION('ref_axis',(0.,0.,-1.));
#7142=DIRECTION('center_axis',(0.,1.,0.));
#7143=DIRECTION('ref_axis',(1.,0.,0.));
#7144=DIRECTION('center_axis',(0.,-1.,0.));
#7145=DIRECTION('ref_axis',(1.,0.,0.));
#7146=DIRECTION('center_axis',(0.,-1.,0.));
#7147=DIRECTION('ref_axis',(0.,0.,-1.));
#7148=DIRECTION('center_axis',(0.,0.,1.));
#7149=DIRECTION('ref_axis',(1.,0.,0.));
#7150=DIRECTION('center_axis',(0.,-1.,0.));
#7151=DIRECTION('ref_axis',(0.,0.,-1.));
#7152=DIRECTION('center_axis',(0.,1.,0.));
#7153=DIRECTION('ref_axis',(1.,0.,0.));
#7154=DIRECTION('center_axis',(0.,-1.,0.));
#7155=DIRECTION('ref_axis',(1.,0.,0.));
#7156=DIRECTION('center_axis',(0.,-1.,0.));
#7157=DIRECTION('ref_axis',(0.,0.,-1.));
#7158=DIRECTION('center_axis',(0.,0.,1.));
#7159=DIRECTION('ref_axis',(1.,0.,0.));
#7160=DIRECTION('center_axis',(0.,-1.,0.));
#7161=DIRECTION('ref_axis',(0.,0.,-1.));
#7162=DIRECTION('center_axis',(0.,1.,0.));
#7163=DIRECTION('ref_axis',(1.,0.,0.));
#7164=DIRECTION('center_axis',(0.,-1.,0.));
#7165=DIRECTION('ref_axis',(1.,0.,0.));
#7166=DIRECTION('center_axis',(0.,-1.,0.));
#7167=DIRECTION('ref_axis',(0.,0.,-1.));
#7168=DIRECTION('center_axis',(0.,0.,1.));
#7169=DIRECTION('ref_axis',(1.,0.,0.));
#7170=DIRECTION('center_axis',(0.,-1.,0.));
#7171=DIRECTION('ref_axis',(0.,0.,-1.));
#7172=DIRECTION('center_axis',(0.,1.,0.));
#7173=DIRECTION('ref_axis',(1.,0.,0.));
#7174=DIRECTION('center_axis',(0.,-1.,0.));
#7175=DIRECTION('ref_axis',(1.,0.,0.));
#7176=DIRECTION('center_axis',(0.,-1.,0.));
#7177=DIRECTION('ref_axis',(0.,0.,-1.));
#7178=DIRECTION('center_axis',(6.12323399573676E-17,0.,1.));
#7179=DIRECTION('ref_axis',(1.,0.,0.));
#7180=DIRECTION('center_axis',(0.,-1.,0.));
#7181=DIRECTION('ref_axis',(0.,0.,-1.));
#7182=DIRECTION('center_axis',(0.,1.,0.));
#7183=DIRECTION('ref_axis',(1.,0.,0.));
#7184=DIRECTION('center_axis',(0.,-1.,0.));
#7185=DIRECTION('ref_axis',(1.,0.,0.));
#7186=DIRECTION('center_axis',(0.,-1.,0.));
#7187=DIRECTION('ref_axis',(0.,0.,-1.));
#7188=DIRECTION('center_axis',(0.,0.,1.));
#7189=DIRECTION('ref_axis',(1.,0.,0.));
#7190=DIRECTION('center_axis',(0.,-1.,0.));
#7191=DIRECTION('ref_axis',(0.,0.,-1.));
#7192=DIRECTION('center_axis',(0.,1.,0.));
#7193=DIRECTION('ref_axis',(1.,0.,0.));
#7194=DIRECTION('center_axis',(0.,1.,0.));
#7195=DIRECTION('ref_axis',(1.,0.,0.));
#7196=DIRECTION('',(0.,1.,0.));
#7197=DIRECTION('center_axis',(0.,-1.,0.));
#7198=DIRECTION('ref_axis',(1.,0.,0.));
#7199=DIRECTION('center_axis',(0.,-1.,0.));
#7200=DIRECTION('ref_axis',(1.,0.,0.));
#7201=DIRECTION('center_axis',(0.,1.,0.));
#7202=DIRECTION('ref_axis',(1.,0.,0.));
#7203=DIRECTION('center_axis',(0.,-1.,0.));
#7204=DIRECTION('ref_axis',(0.,0.,-1.));
#7205=DIRECTION('center_axis',(0.,0.,1.));
#7206=DIRECTION('ref_axis',(1.,0.,0.));
#7207=DIRECTION('center_axis',(0.,-1.,0.));
#7208=DIRECTION('ref_axis',(0.,0.,-1.));
#7209=DIRECTION('center_axis',(0.,-1.,0.));
#7210=DIRECTION('ref_axis',(-1.,0.,0.));
#7211=DIRECTION('center_axis',(0.,1.,0.));
#7212=DIRECTION('ref_axis',(1.,0.,0.));
#7213=DIRECTION('axis',(0.,0.,1.));
#7214=DIRECTION('refdir',(1.,0.,0.));
#7215=DIRECTION('center_axis',(0.,1.,0.));
#7216=DIRECTION('ref_axis',(0.,0.,1.));
#7217=DIRECTION('center_axis',(0.,-1.,0.));
#7218=DIRECTION('ref_axis',(1.,0.,0.));
#7219=DIRECTION('center_axis',(0.,-1.,0.));
#7220=DIRECTION('ref_axis',(1.,0.,0.));
#7221=DIRECTION('center_axis',(0.,-1.,0.));
#7222=DIRECTION('ref_axis',(1.,0.,0.));
#7223=DIRECTION('center_axis',(0.,-1.,0.));
#7224=DIRECTION('ref_axis',(1.,0.,0.));
#7225=DIRECTION('',(0.,1.,0.));
#7226=DIRECTION('center_axis',(0.,-1.,0.));
#7227=DIRECTION('ref_axis',(0.,0.,-1.));
#7228=DIRECTION('center_axis',(0.,-1.,0.));
#7229=DIRECTION('ref_axis',(1.,0.,0.));
#7230=DIRECTION('center_axis',(0.,-1.,0.));
#7231=DIRECTION('ref_axis',(1.,0.,0.));
#7232=DIRECTION('',(0.,1.,0.));
#7233=DIRECTION('center_axis',(0.,1.,0.));
#7234=DIRECTION('ref_axis',(0.,0.,1.));
#7235=DIRECTION('center_axis',(0.,-1.,0.));
#7236=DIRECTION('ref_axis',(1.,0.,0.));
#7237=DIRECTION('center_axis',(0.,-1.,0.));
#7238=DIRECTION('ref_axis',(1.,0.,0.));
#7239=DIRECTION('center_axis',(0.,-1.,0.));
#7240=DIRECTION('ref_axis',(1.,0.,0.));
#7241=DIRECTION('center_axis',(0.,-1.,0.));
#7242=DIRECTION('ref_axis',(1.,0.,0.));
#7243=DIRECTION('',(0.,1.,0.));
#7244=DIRECTION('center_axis',(0.,-1.,0.));
#7245=DIRECTION('ref_axis',(0.,0.,-1.));
#7246=DIRECTION('center_axis',(0.,-1.,0.));
#7247=DIRECTION('ref_axis',(1.,0.,0.));
#7248=DIRECTION('center_axis',(0.,-1.,0.));
#7249=DIRECTION('ref_axis',(1.,0.,0.));
#7250=DIRECTION('',(0.,1.,0.));
#7251=DIRECTION('',(0.,0.,1.));
#7252=DIRECTION('',(1.,0.,0.));
#7253=DIRECTION('',(0.,0.,1.));
#7254=DIRECTION('',(1.,0.,0.));
#7255=DIRECTION('',(0.,0.,1.));
#7256=DIRECTION('',(1.,0.,0.));
#7257=DIRECTION('',(0.,0.,1.));
#7258=DIRECTION('',(1.,0.,0.));
#7259=DIRECTION('',(0.,0.,1.));
#7260=DIRECTION('',(1.,0.,0.));
#7261=DIRECTION('axis',(0.,0.,1.));
#7262=DIRECTION('refdir',(1.,0.,0.));
#7263=DIRECTION('center_axis',(0.866025403784439,0.,-0.5));
#7264=DIRECTION('ref_axis',(0.5,0.,0.866025403784439));
#7265=DIRECTION('',(-0.5,0.,-0.866025403784439));
#7266=DIRECTION('',(0.,-1.,0.));
#7267=DIRECTION('',(0.5,0.,0.866025403784439));
#7268=DIRECTION('',(0.,-1.,0.));
#7269=DIRECTION('center_axis',(1.60246890531964E-16,0.,-1.));
#7270=DIRECTION('ref_axis',(1.,0.,1.60246890531964E-16));
#7271=DIRECTION('',(-1.,0.,-1.60246890531964E-16));
#7272=DIRECTION('',(0.,-1.,0.));
#7273=DIRECTION('',(1.,0.,1.60246890531964E-16));
#7274=DIRECTION('center_axis',(-0.866025403784439,0.,-0.5));
#7275=DIRECTION('ref_axis',(0.5,0.,-0.866025403784439));
#7276=DIRECTION('',(-0.5,0.,0.866025403784439));
#7277=DIRECTION('',(0.,-1.,0.));
#7278=DIRECTION('',(0.5,0.,-0.866025403784439));
#7279=DIRECTION('center_axis',(-0.866025403784439,0.,0.5));
#7280=DIRECTION('ref_axis',(-0.5,0.,-0.866025403784439));
#7281=DIRECTION('',(0.5,0.,0.866025403784439));
#7282=DIRECTION('',(0.,-1.,0.));
#7283=DIRECTION('',(-0.5,0.,-0.866025403784439));
#7284=DIRECTION('center_axis',(-1.60246890531964E-16,0.,1.));
#7285=DIRECTION('ref_axis',(-1.,0.,-1.60246890531964E-16));
#7286=DIRECTION('',(1.,0.,1.60246890531964E-16));
#7287=DIRECTION('',(0.,-1.,0.));
#7288=DIRECTION('',(-1.,0.,-1.60246890531964E-16));
#7289=DIRECTION('center_axis',(0.866025403784439,0.,0.5));
#7290=DIRECTION('ref_axis',(-0.5,0.,0.866025403784439));
#7291=DIRECTION('',(0.5,0.,-0.866025403784439));
#7292=DIRECTION('',(-0.5,0.,0.866025403784439));
#7293=DIRECTION('center_axis',(0.,1.,0.));
#7294=DIRECTION('ref_axis',(1.,0.,0.));
#7295=DIRECTION('center_axis',(0.,-1.,0.));
#7296=DIRECTION('ref_axis',(0.,0.,-1.));
#7297=DIRECTION('center_axis',(0.,1.,0.));
#7298=DIRECTION('ref_axis',(1.,0.,0.));
#7299=DIRECTION('center_axis',(0.,1.,0.));
#7300=DIRECTION('ref_axis',(1.,0.,0.));
#7301=DIRECTION('center_axis',(0.,1.,0.));
#7302=DIRECTION('ref_axis',(0.,0.,1.));
#7303=DIRECTION('center_axis',(0.,-1.,0.));
#7304=DIRECTION('ref_axis',(1.,0.,0.));
#7305=DIRECTION('center_axis',(0.,-1.,0.));
#7306=DIRECTION('ref_axis',(1.,0.,0.));
#7307=DIRECTION('center_axis',(0.,-1.,0.));
#7308=DIRECTION('ref_axis',(1.,0.,0.));
#7309=DIRECTION('',(0.707106781186547,0.707106781186548,8.65956056235493E-17));
#7310=DIRECTION('center_axis',(0.,-1.,0.));
#7311=DIRECTION('ref_axis',(1.,0.,0.));
#7312=DIRECTION('center_axis',(0.,-1.,0.));
#7313=DIRECTION('ref_axis',(1.,0.,0.));
#7314=DIRECTION('',(0.,1.,0.));
#7315=DIRECTION('center_axis',(0.,1.,0.));
#7316=DIRECTION('ref_axis',(1.,0.,0.));
#7317=DIRECTION('center_axis',(0.,-1.,0.));
#7318=DIRECTION('ref_axis',(1.,0.,0.));
#7319=DIRECTION('',(-0.707106781186547,0.707106781186548,-8.65956056235493E-17));
#7320=DIRECTION('center_axis',(0.,-1.,0.));
#7321=DIRECTION('ref_axis',(0.,0.,-1.));
#7322=DIRECTION('center_axis',(0.,-1.,0.));
#7323=DIRECTION('ref_axis',(1.,0.,0.));
#7324=DIRECTION('center_axis',(0.,1.,0.));
#7325=DIRECTION('ref_axis',(1.,0.,0.));
#7326=DIRECTION('center_axis',(0.,1.,0.));
#7327=DIRECTION('ref_axis',(1.,0.,0.));
#7328=DIRECTION('',(-0.447213595499958,0.894427190999916,-5.47678698264203E-17));
#7329=DIRECTION('center_axis',(0.,-1.,0.));
#7330=DIRECTION('ref_axis',(1.,0.,0.));
#7331=DIRECTION('',(0.,1.,0.));
#7332=DIRECTION('',(0.,0.,1.));
#7333=DIRECTION('',(1.,0.,0.));
#7334=DIRECTION('',(0.,0.,1.));
#7335=DIRECTION('',(1.,0.,0.));
#7336=DIRECTION('',(0.,0.,1.));
#7337=DIRECTION('',(1.,0.,0.));
#7338=DIRECTION('',(0.,0.,1.));
#7339=DIRECTION('',(1.,0.,0.));
#7340=DIRECTION('',(0.,0.,1.));
#7341=DIRECTION('',(1.,0.,0.));
#7342=DIRECTION('',(0.,0.,1.));
#7343=DIRECTION('',(1.,0.,0.));
#7344=DIRECTION('',(0.,0.,1.));
#7345=DIRECTION('',(-1.,1.22464679914735E-16,0.));
#7346=DIRECTION('',(0.,0.,1.));
#7347=DIRECTION('',(-1.,1.22464679914735E-16,0.));
#7348=DIRECTION('',(0.,0.,1.));
#7349=DIRECTION('',(-1.,1.22464679914735E-16,0.));
#7350=DIRECTION('',(0.,0.,1.));
#7351=DIRECTION('',(-1.,1.22464679914735E-16,0.));
#7352=DIRECTION('',(0.,0.,1.));
#7353=DIRECTION('',(1.,0.,0.));
#7354=DIRECTION('',(0.,0.,1.));
#7355=DIRECTION('',(1.,0.,0.));
#7356=DIRECTION('',(0.,0.,1.));
#7357=DIRECTION('',(1.,0.,0.));
#7358=DIRECTION('',(0.,0.,1.));
#7359=DIRECTION('',(1.,0.,0.));
#7360=DIRECTION('axis',(0.,0.,1.));
#7361=DIRECTION('refdir',(1.,0.,0.));
#7362=DIRECTION('axis',(0.,0.,1.));
#7363=DIRECTION('refdir',(1.,0.,0.));
#7364=DIRECTION('center_axis',(0.,0.,1.));
#7365=DIRECTION('ref_axis',(1.,0.,0.));
#7366=DIRECTION('center_axis',(0.,0.,1.));
#7367=DIRECTION('ref_axis',(1.,0.,0.));
#7368=DIRECTION('center_axis',(0.,0.,1.));
#7369=DIRECTION('ref_axis',(1.,0.,0.));
#7370=DIRECTION('center_axis',(0.,0.,1.));
#7371=DIRECTION('ref_axis',(1.,0.,0.));
#7372=DIRECTION('center_axis',(0.,0.,1.));
#7373=DIRECTION('ref_axis',(1.,0.,0.));
#7374=DIRECTION('center_axis',(0.,0.,-1.));
#7375=DIRECTION('ref_axis',(1.,0.,0.));
#7376=DIRECTION('center_axis',(0.,0.,1.));
#7377=DIRECTION('ref_axis',(1.,0.,0.));
#7378=DIRECTION('',(0.,0.,-1.));
#7379=DIRECTION('center_axis',(0.,0.,1.));
#7380=DIRECTION('ref_axis',(1.,0.,0.));
#7381=DIRECTION('',(0.,0.,-1.));
#7382=DIRECTION('center_axis',(0.,0.,-1.));
#7383=DIRECTION('ref_axis',(1.,0.,0.));
#7384=DIRECTION('center_axis',(0.,0.,-1.));
#7385=DIRECTION('ref_axis',(1.,0.,0.));
#7386=DIRECTION('center_axis',(0.,0.,-1.));
#7387=DIRECTION('ref_axis',(1.,0.,0.));
#7388=DIRECTION('center_axis',(0.,0.,1.));
#7389=DIRECTION('ref_axis',(1.,0.,0.));
#7390=DIRECTION('center_axis',(0.,0.,1.));
#7391=DIRECTION('ref_axis',(1.,0.,0.));
#7392=DIRECTION('',(0.,0.,-1.));
#7393=DIRECTION('center_axis',(0.,0.,1.));
#7394=DIRECTION('ref_axis',(1.,0.,0.));
#7395=DIRECTION('center_axis',(0.,0.,1.));
#7396=DIRECTION('ref_axis',(1.,0.,0.));
#7397=DIRECTION('',(-1.,0.,0.));
#7398=DIRECTION('',(0.,1.,0.));
#7399=DIRECTION('',(1.,0.,0.));
#7400=DIRECTION('center_axis',(0.,0.,1.));
#7401=DIRECTION('ref_axis',(1.,0.,0.));
#7402=DIRECTION('',(1.,0.,0.));
#7403=DIRECTION('',(0.,1.,0.));
#7404=DIRECTION('',(-1.,0.,0.));
#7405=DIRECTION('center_axis',(-1.,0.,0.));
#7406=DIRECTION('ref_axis',(0.,0.,1.));
#7407=DIRECTION('',(0.,1.,0.));
#7408=DIRECTION('',(0.,0.,-1.));
#7409=DIRECTION('',(0.,0.,1.));
#7410=DIRECTION('center_axis',(0.,0.,-1.));
#7411=DIRECTION('ref_axis',(-1.,0.,0.));
#7412=DIRECTION('',(0.,-1.,0.));
#7413=DIRECTION('',(-1.,0.,0.));
#7414=DIRECTION('',(0.,1.,0.));
#7415=DIRECTION('',(1.,0.,0.));
#7416=DIRECTION('center_axis',(0.,1.,0.));
#7417=DIRECTION('ref_axis',(1.,0.,0.));
#7418=DIRECTION('',(0.,0.,-1.));
#7419=DIRECTION('center_axis',(0.,-1.,0.));
#7420=DIRECTION('ref_axis',(1.,0.,0.));
#7421=DIRECTION('',(1.,0.,0.));
#7422=DIRECTION('center_axis',(0.,1.,0.));
#7423=DIRECTION('ref_axis',(1.,0.,0.));
#7424=DIRECTION('center_axis',(0.,1.,0.));
#7425=DIRECTION('ref_axis',(1.,0.,0.));
#7426=DIRECTION('center_axis',(0.,-1.,0.));
#7427=DIRECTION('ref_axis',(1.,0.,0.));
#7428=DIRECTION('',(0.,1.,0.));
#7429=DIRECTION('center_axis',(0.,1.,0.));
#7430=DIRECTION('ref_axis',(1.,0.,0.));
#7431=DIRECTION('',(0.,0.,1.));
#7432=DIRECTION('center_axis',(0.,1.,0.));
#7433=DIRECTION('ref_axis',(1.,0.,0.));
#7434=DIRECTION('',(-1.,0.,0.));
#7435=DIRECTION('center_axis',(-1.,0.,0.));
#7436=DIRECTION('ref_axis',(0.,0.,1.));
#7437=DIRECTION('center_axis',(0.,0.,-1.));
#7438=DIRECTION('ref_axis',(-1.,0.,0.));
#7439=DIRECTION('',(0.,-1.,0.));
#7440=DIRECTION('center_axis',(0.,1.,0.));
#7441=DIRECTION('ref_axis',(-0.267261241912424,0.,-0.963624111659432));
#7442=DIRECTION('axis',(0.,0.,1.));
#7443=DIRECTION('refdir',(1.,0.,0.));
#7444=DIRECTION('center_axis',(0.,0.,1.));
#7445=DIRECTION('ref_axis',(1.,0.,0.));
#7446=DIRECTION('center_axis',(0.,0.,-1.));
#7447=DIRECTION('ref_axis',(1.,0.,0.));
#7448=DIRECTION('',(0.,0.,-1.));
#7449=DIRECTION('center_axis',(0.,0.,-1.));
#7450=DIRECTION('ref_axis',(1.,0.,0.));
#7451=DIRECTION('center_axis',(0.,0.,1.));
#7452=DIRECTION('ref_axis',(1.,0.,0.));
#7453=DIRECTION('center_axis',(0.,0.,1.));
#7454=DIRECTION('ref_axis',(1.,0.,0.));
#7455=DIRECTION('',(0.,0.,-1.));
#7456=DIRECTION('center_axis',(0.,0.,1.));
#7457=DIRECTION('ref_axis',(1.,0.,0.));
#7458=DIRECTION('center_axis',(0.,0.,1.));
#7459=DIRECTION('ref_axis',(1.,0.,0.));
#7460=DIRECTION('center_axis',(0.,0.,1.));
#7461=DIRECTION('ref_axis',(1.,0.,0.));
#7462=DIRECTION('axis',(0.,0.,1.));
#7463=DIRECTION('refdir',(1.,0.,0.));
#7464=DIRECTION('center_axis',(0.,0.,1.));
#7465=DIRECTION('ref_axis',(1.,0.,0.));
#7466=DIRECTION('center_axis',(0.,0.,1.));
#7467=DIRECTION('ref_axis',(1.,0.,0.));
#7468=DIRECTION('',(0.,0.,1.));
#7469=DIRECTION('center_axis',(0.,0.,-1.));
#7470=DIRECTION('ref_axis',(1.,0.,0.));
#7471=DIRECTION('center_axis',(-1.60246890531964E-16,-1.,0.));
#7472=DIRECTION('ref_axis',(1.,-1.60246890531964E-16,0.));
#7473=DIRECTION('',(1.,-1.60246890531964E-16,0.));
#7474=DIRECTION('',(0.,0.,1.));
#7475=DIRECTION('',(1.,-1.60246890531964E-16,0.));
#7476=DIRECTION('',(0.,0.,1.));
#7477=DIRECTION('center_axis',(-0.866025403784439,-0.5,0.));
#7478=DIRECTION('ref_axis',(0.5,-0.866025403784439,0.));
#7479=DIRECTION('',(0.5,-0.866025403784439,0.));
#7480=DIRECTION('',(0.5,-0.866025403784439,0.));
#7481=DIRECTION('',(0.,0.,1.));
#7482=DIRECTION('center_axis',(-0.866025403784439,0.5,0.));
#7483=DIRECTION('ref_axis',(-0.5,-0.866025403784439,0.));
#7484=DIRECTION('',(-0.5,-0.866025403784439,0.));
#7485=DIRECTION('',(-0.5,-0.866025403784439,0.));
#7486=DIRECTION('',(0.,0.,1.));
#7487=DIRECTION('center_axis',(1.60246890531964E-16,1.,0.));
#7488=DIRECTION('ref_axis',(-1.,1.60246890531964E-16,0.));
#7489=DIRECTION('',(-1.,1.60246890531964E-16,0.));
#7490=DIRECTION('',(-1.,1.60246890531964E-16,0.));
#7491=DIRECTION('',(0.,0.,1.));
#7492=DIRECTION('center_axis',(0.866025403784439,0.5,0.));
#7493=DIRECTION('ref_axis',(-0.5,0.866025403784439,0.));
#7494=DIRECTION('',(-0.5,0.866025403784439,0.));
#7495=DIRECTION('',(-0.5,0.866025403784439,0.));
#7496=DIRECTION('',(0.,0.,1.));
#7497=DIRECTION('center_axis',(0.866025403784439,-0.5,0.));
#7498=DIRECTION('ref_axis',(0.5,0.866025403784439,0.));
#7499=DIRECTION('',(0.5,0.866025403784439,0.));
#7500=DIRECTION('',(0.5,0.866025403784439,0.));
#7501=DIRECTION('center_axis',(0.,0.,1.));
#7502=DIRECTION('ref_axis',(1.,0.,0.));
#7503=DIRECTION('center_axis',(0.,0.,1.));
#7504=DIRECTION('ref_axis',(1.,0.,0.));
#7505=DIRECTION('',(0.,0.,1.));
#7506=DIRECTION('',(1.,0.,0.));
#7507=DIRECTION('',(0.,0.,1.));
#7508=DIRECTION('',(1.,0.,0.));
#7509=DIRECTION('',(0.,0.,1.));
#7510=DIRECTION('',(1.,0.,0.));
#7511=DIRECTION('axis',(0.,0.,1.));
#7512=DIRECTION('refdir',(1.,0.,0.));
#7513=DIRECTION('axis',(0.,0.,1.));
#7514=DIRECTION('refdir',(1.,0.,0.));
#7515=DIRECTION('center_axis',(0.,1.,0.));
#7516=DIRECTION('ref_axis',(1.,0.,0.));
#7517=DIRECTION('center_axis',(0.,1.,0.));
#7518=DIRECTION('ref_axis',(1.,0.,0.));
#7519=DIRECTION('',(0.,1.,0.));
#7520=DIRECTION('center_axis',(0.,-1.,0.));
#7521=DIRECTION('ref_axis',(1.,0.,0.));
#7522=DIRECTION('center_axis',(0.,1.,0.));
#7523=DIRECTION('ref_axis',(1.,0.,0.));
#7524=DIRECTION('center_axis',(0.,1.,0.));
#7525=DIRECTION('ref_axis',(1.,0.,0.));
#7526=DIRECTION('',(0.,1.,0.));
#7527=DIRECTION('center_axis',(0.,-1.,0.));
#7528=DIRECTION('ref_axis',(1.,0.,0.));
#7529=DIRECTION('center_axis',(0.,1.,0.));
#7530=DIRECTION('ref_axis',(-1.83697019872103E-16,0.,1.));
#7531=DIRECTION('',(0.,1.,0.));
#7532=DIRECTION('center_axis',(0.,1.,0.));
#7533=DIRECTION('ref_axis',(1.,0.,0.));
#7534=DIRECTION('',(0.,-1.,0.));
#7535=DIRECTION('center_axis',(0.,1.,0.));
#7536=DIRECTION('ref_axis',(1.,0.,0.));
#7537=DIRECTION('center_axis',(0.,1.,0.));
#7538=DIRECTION('ref_axis',(1.,0.,0.));
#7539=DIRECTION('center_axis',(0.,1.,0.));
#7540=DIRECTION('ref_axis',(1.,0.,0.));
#7541=DIRECTION('center_axis',(0.,1.,0.));
#7542=DIRECTION('ref_axis',(-1.83697019872103E-16,0.,-1.));
#7543=DIRECTION('center_axis',(0.,1.,0.));
#7544=DIRECTION('ref_axis',(1.,0.,0.));
#7545=DIRECTION('center_axis',(0.,1.,0.));
#7546=DIRECTION('ref_axis',(1.,0.,0.));
#7547=DIRECTION('',(0.,0.,1.));
#7548=DIRECTION('',(1.,0.,0.));
#7549=DIRECTION('',(0.,0.,1.));
#7550=DIRECTION('',(1.,0.,0.));
#7551=DIRECTION('',(0.,0.,1.));
#7552=DIRECTION('',(1.,0.,0.));
#7553=DIRECTION('',(0.,0.,1.));
#7554=DIRECTION('',(1.,0.,0.));
#7555=DIRECTION('',(0.,0.,1.));
#7556=DIRECTION('',(1.,0.,0.));
#7557=CARTESIAN_POINT('',(0.,0.,0.));
#7558=CARTESIAN_POINT('',(0.,0.,0.));
#7559=CARTESIAN_POINT('',(0.,0.,0.));
#7560=CARTESIAN_POINT('Origin',(0.,-2.8,12.));
#7561=CARTESIAN_POINT('',(-2.99903459153175,-2.8,10.7476855351806));
#7562=CARTESIAN_POINT('',(-2.60150387000671,-2.8,10.0520067725117));
#7563=CARTESIAN_POINT('Origin',(-3.5,-2.8,10.));
#7564=CARTESIAN_POINT('',(-2.99903459153175,-2.8,13.2523144648194));
#7565=CARTESIAN_POINT('Origin',(0.,-2.8,12.));
#7566=CARTESIAN_POINT('',(-2.60150387000671,-2.8,13.9479932274883));
#7567=CARTESIAN_POINT('Origin',(-3.5,-2.8,14.));
#7568=CARTESIAN_POINT('',(2.60150387000671,-2.8,13.9479932274883));
#7569=CARTESIAN_POINT('Origin',(0.,-2.8,12.));
#7570=CARTESIAN_POINT('',(2.99903459153175,-2.8,13.2523144648194));
#7571=CARTESIAN_POINT('Origin',(3.5,-2.8,14.));
#7572=CARTESIAN_POINT('',(2.99903459153175,-2.8,10.7476855351806));
#7573=CARTESIAN_POINT('Origin',(0.,-2.8,12.));
#7574=CARTESIAN_POINT('',(2.60150387000671,-2.8,10.0520067725117));
#7575=CARTESIAN_POINT('Origin',(3.5,-2.8,10.));
#7576=CARTESIAN_POINT('Origin',(0.,-2.8,12.));
#7577=CARTESIAN_POINT('',(-1.2,-2.8,12.));
#7578=CARTESIAN_POINT('Origin',(0.,-2.8,12.));
#7579=CARTESIAN_POINT('Origin',(0.,-2.8,12.));
#7580=CARTESIAN_POINT('',(2.99903459153175,-2.5,10.7476855351806));
#7581=CARTESIAN_POINT('',(2.99903459153175,-2.8,10.7476855351806));
#7582=CARTESIAN_POINT('',(2.99903459153175,-2.5,13.2523144648194));
#7583=CARTESIAN_POINT('',(2.99903459153175,-2.8,13.2523144648194));
#7584=CARTESIAN_POINT('Origin',(0.,-2.5,12.));
#7585=CARTESIAN_POINT('Origin',(0.,-2.8,12.));
#7586=CARTESIAN_POINT('',(-2.60150387000671,-2.5,13.9479932274883));
#7587=CARTESIAN_POINT('',(-2.60150387000671,-2.8,13.9479932274883));
#7588=CARTESIAN_POINT('',(2.60150387000671,-2.5,13.9479932274883));
#7589=CARTESIAN_POINT('Origin',(0.,-2.5,12.));
#7590=CARTESIAN_POINT('',(2.60150387000671,-2.8,13.9479932274883));
#7591=CARTESIAN_POINT('Origin',(0.,-2.8,12.));
#7592=CARTESIAN_POINT('',(-2.60150387000671,-2.5,10.0520067725117));
#7593=CARTESIAN_POINT('',(-2.60150387000671,-2.8,10.0520067725117));
#7594=CARTESIAN_POINT('',(2.60150387000671,-2.5,10.0520067725117));
#7595=CARTESIAN_POINT('',(2.60150387000671,-2.8,10.0520067725117));
#7596=CARTESIAN_POINT('Origin',(0.,-2.5,12.));
#7597=CARTESIAN_POINT('Origin',(0.,-2.8,12.));
#7598=CARTESIAN_POINT('',(-1.2,-2.5,12.));
#7599=CARTESIAN_POINT('',(-1.2,-2.8,12.));
#7600=CARTESIAN_POINT('Origin',(0.,-2.5,12.));
#7601=CARTESIAN_POINT('Origin',(0.,-2.8,12.));
#7602=CARTESIAN_POINT('',(-2.99903459153175,-2.5,10.7476855351806));
#7603=CARTESIAN_POINT('',(-2.99903459153175,-2.8,10.7476855351806));
#7604=CARTESIAN_POINT('',(-2.99903459153175,-2.5,13.2523144648194));
#7605=CARTESIAN_POINT('Origin',(0.,-2.5,12.));
#7606=CARTESIAN_POINT('',(-2.99903459153175,-2.8,13.2523144648194));
#7607=CARTESIAN_POINT('Origin',(-3.5,-3.2,10.));
#7608=CARTESIAN_POINT('',(-4.4,-3.1,10.));
#7609=CARTESIAN_POINT('Origin',(-3.5,-3.1,10.));
#7610=CARTESIAN_POINT('',(-4.4,-2.5,10.));
#7611=CARTESIAN_POINT('',(-4.4,-3.2,10.));
#7612=CARTESIAN_POINT('Origin',(-3.5,-2.5,10.));
#7613=CARTESIAN_POINT('Origin',(-3.5,-2.5,10.));
#7614=CARTESIAN_POINT('Origin',(3.5,-3.2,10.));
#7615=CARTESIAN_POINT('',(2.6,-3.1,10.));
#7616=CARTESIAN_POINT('Origin',(3.5,-3.1,10.));
#7617=CARTESIAN_POINT('',(2.6,-2.5,10.));
#7618=CARTESIAN_POINT('',(2.6,-3.2,10.));
#7619=CARTESIAN_POINT('Origin',(3.5,-2.5,10.));
#7620=CARTESIAN_POINT('Origin',(3.5,-2.5,10.));
#7621=CARTESIAN_POINT('Origin',(3.5,-3.2,14.));
#7622=CARTESIAN_POINT('',(2.6,-3.1,14.));
#7623=CARTESIAN_POINT('Origin',(3.5,-3.1,14.));
#7624=CARTESIAN_POINT('',(2.6,-2.5,14.));
#7625=CARTESIAN_POINT('',(2.6,-3.2,14.));
#7626=CARTESIAN_POINT('Origin',(3.5,-2.5,14.));
#7627=CARTESIAN_POINT('Origin',(3.5,-2.5,14.));
#7628=CARTESIAN_POINT('Origin',(0.,-2.5,13.25));
#7629=CARTESIAN_POINT('',(-1.,-2.5,12.));
#7630=CARTESIAN_POINT('Origin',(0.,-2.5,12.));
#7631=CARTESIAN_POINT('Origin',(-3.5,-3.2,14.));
#7632=CARTESIAN_POINT('',(-4.4,-3.1,14.));
#7633=CARTESIAN_POINT('Origin',(-3.5,-3.1,14.));
#7634=CARTESIAN_POINT('',(-4.4,-2.5,14.));
#7635=CARTESIAN_POINT('',(-4.4,-3.2,14.));
#7636=CARTESIAN_POINT('Origin',(-3.5,-2.5,14.));
#7637=CARTESIAN_POINT('Origin',(-3.5,-2.5,14.));
#7638=CARTESIAN_POINT('Origin',(-2.,-3.2,5.));
#7639=CARTESIAN_POINT('',(-2.425,-3.1,5.));
#7640=CARTESIAN_POINT('Origin',(-2.,-3.1,5.));
#7641=CARTESIAN_POINT('',(-2.425,-2.5,5.));
#7642=CARTESIAN_POINT('',(-2.425,-3.2,5.));
#7643=CARTESIAN_POINT('Origin',(-2.,-2.5,5.));
#7644=CARTESIAN_POINT('Origin',(2.,-3.2,5.));
#7645=CARTESIAN_POINT('',(1.575,-3.1,5.));
#7646=CARTESIAN_POINT('Origin',(2.,-3.1,5.));
#7647=CARTESIAN_POINT('',(1.575,-2.5,5.));
#7648=CARTESIAN_POINT('',(1.575,-3.2,5.));
#7649=CARTESIAN_POINT('Origin',(2.,-2.5,5.));
#7650=CARTESIAN_POINT('Origin',(0.,-3.2,20.5));
#7651=CARTESIAN_POINT('',(-0.425,-3.1,20.5));
#7652=CARTESIAN_POINT('Origin',(0.,-3.1,20.5));
#7653=CARTESIAN_POINT('',(-0.425,-2.5,20.5));
#7654=CARTESIAN_POINT('',(-0.425,-3.2,20.5));
#7655=CARTESIAN_POINT('Origin',(0.,-2.5,20.5));
#7656=CARTESIAN_POINT('Origin',(0.,-3.2,12.));
#7657=CARTESIAN_POINT('',(-1.,-3.1,12.));
#7658=CARTESIAN_POINT('Origin',(0.,-3.1,12.));
#7659=CARTESIAN_POINT('',(-1.,-3.2,12.));
#7660=CARTESIAN_POINT('Origin',(-3.,-3.1,4.5));
#7661=CARTESIAN_POINT('',(-6.,-3.1,9.));
#7662=CARTESIAN_POINT('',(-3.,-3.1,4.5));
#7663=CARTESIAN_POINT('',(-6.,-3.1,9.));
#7664=CARTESIAN_POINT('',(-6.,-2.5,9.));
#7665=CARTESIAN_POINT('',(-6.,-3.1,9.));
#7666=CARTESIAN_POINT('',(-3.,-2.5,4.5));
#7667=CARTESIAN_POINT('',(-6.,-2.5,9.));
#7668=CARTESIAN_POINT('',(-3.,-3.1,4.5));
#7669=CARTESIAN_POINT('Origin',(3.,-3.1,4.5));
#7670=CARTESIAN_POINT('',(3.,-3.1,4.5));
#7671=CARTESIAN_POINT('',(-3.,-3.1,4.5));
#7672=CARTESIAN_POINT('',(3.,-2.5,4.5));
#7673=CARTESIAN_POINT('',(-3.,-2.5,4.5));
#7674=CARTESIAN_POINT('',(3.,-3.1,4.5));
#7675=CARTESIAN_POINT('Origin',(6.,-3.1,9.));
#7676=CARTESIAN_POINT('',(6.,-3.1,9.));
#7677=CARTESIAN_POINT('',(3.,-3.1,4.5));
#7678=CARTESIAN_POINT('',(6.,-2.5,9.));
#7679=CARTESIAN_POINT('',(3.,-2.5,4.5));
#7680=CARTESIAN_POINT('',(6.,-3.1,9.));
#7681=CARTESIAN_POINT('Origin',(6.,-3.1,15.));
#7682=CARTESIAN_POINT('',(6.,-3.1,15.));
#7683=CARTESIAN_POINT('',(6.,-3.1,9.));
#7684=CARTESIAN_POINT('',(6.,-2.5,15.));
#7685=CARTESIAN_POINT('',(6.,-2.5,9.));
#7686=CARTESIAN_POINT('',(6.,-3.1,15.));
#7687=CARTESIAN_POINT('Origin',(2.5,-3.1,22.));
#7688=CARTESIAN_POINT('',(2.5,-3.1,22.));
#7689=CARTESIAN_POINT('',(6.,-3.1,15.));
#7690=CARTESIAN_POINT('',(2.5,-2.5,22.));
#7691=CARTESIAN_POINT('',(6.,-2.5,15.));
#7692=CARTESIAN_POINT('',(2.5,-3.1,22.));
#7693=CARTESIAN_POINT('Origin',(-2.5,-3.1,22.));
#7694=CARTESIAN_POINT('',(-2.5,-3.1,22.));
#7695=CARTESIAN_POINT('',(2.5,-3.1,22.));
#7696=CARTESIAN_POINT('',(-2.5,-2.5,22.));
#7697=CARTESIAN_POINT('',(2.5,-2.5,22.));
#7698=CARTESIAN_POINT('',(-2.5,-3.1,22.));
#7699=CARTESIAN_POINT('Origin',(-6.,-3.1,15.));
#7700=CARTESIAN_POINT('',(-6.,-3.1,15.));
#7701=CARTESIAN_POINT('',(-2.5,-3.1,22.));
#7702=CARTESIAN_POINT('',(-6.,-2.5,15.));
#7703=CARTESIAN_POINT('',(-2.5,-2.5,22.));
#7704=CARTESIAN_POINT('',(-6.,-3.1,15.));
#7705=CARTESIAN_POINT('Origin',(-6.,-3.1,9.));
#7706=CARTESIAN_POINT('',(-6.,-3.1,15.));
#7707=CARTESIAN_POINT('',(-6.,-2.5,15.));
#7708=CARTESIAN_POINT('Origin',(0.,-2.5,13.25));
#7709=CARTESIAN_POINT('Origin',(0.,-3.1,13.25));
#7710=CARTESIAN_POINT('',(0.,0.,0.));
#7711=CARTESIAN_POINT('Origin',(0.,2.8,12.));
#7712=CARTESIAN_POINT('',(-2.60150387000671,2.8,10.0520067725117));
#7713=CARTESIAN_POINT('',(-2.99903459153175,2.8,10.7476855351806));
#7714=CARTESIAN_POINT('Origin',(-3.5,2.8,10.));
#7715=CARTESIAN_POINT('',(2.60150387000671,2.8,10.0520067725117));
#7716=CARTESIAN_POINT('Origin',(0.,2.8,12.));
#7717=CARTESIAN_POINT('',(2.99903459153175,2.8,10.7476855351806));
#7718=CARTESIAN_POINT('Origin',(3.5,2.8,10.));
#7719=CARTESIAN_POINT('',(2.99903459153175,2.8,13.2523144648194));
#7720=CARTESIAN_POINT('Origin',(0.,2.8,12.));
#7721=CARTESIAN_POINT('',(2.60150387000671,2.8,13.9479932274883));
#7722=CARTESIAN_POINT('Origin',(3.5,2.8,14.));
#7723=CARTESIAN_POINT('',(-2.60150387000671,2.8,13.9479932274883));
#7724=CARTESIAN_POINT('Origin',(0.,2.8,12.));
#7725=CARTESIAN_POINT('',(-2.99903459153175,2.8,13.2523144648194));
#7726=CARTESIAN_POINT('Origin',(-3.5,2.8,14.));
#7727=CARTESIAN_POINT('Origin',(0.,2.8,12.));
#7728=CARTESIAN_POINT('',(-1.2,2.8,12.));
#7729=CARTESIAN_POINT('Origin',(0.,2.8,12.));
#7730=CARTESIAN_POINT('Origin',(0.,2.5,12.));
#7731=CARTESIAN_POINT('',(-2.60150387000671,2.5,13.9479932274883));
#7732=CARTESIAN_POINT('',(-2.60150387000671,2.5,13.9479932274883));
#7733=CARTESIAN_POINT('',(2.60150387000671,2.5,13.9479932274883));
#7734=CARTESIAN_POINT('',(2.60150387000671,2.5,13.9479932274883));
#7735=CARTESIAN_POINT('Origin',(0.,2.5,12.));
#7736=CARTESIAN_POINT('Origin',(0.,2.5,12.));
#7737=CARTESIAN_POINT('',(-2.99903459153175,2.5,10.7476855351806));
#7738=CARTESIAN_POINT('',(-2.99903459153175,2.5,10.7476855351806));
#7739=CARTESIAN_POINT('',(-2.99903459153175,2.5,13.2523144648194));
#7740=CARTESIAN_POINT('',(-2.99903459153175,2.5,13.2523144648194));
#7741=CARTESIAN_POINT('Origin',(0.,2.5,12.));
#7742=CARTESIAN_POINT('Origin',(0.,2.5,12.));
#7743=CARTESIAN_POINT('',(2.99903459153175,2.5,10.7476855351806));
#7744=CARTESIAN_POINT('',(2.99903459153175,2.5,10.7476855351806));
#7745=CARTESIAN_POINT('',(2.99903459153175,2.5,13.2523144648194));
#7746=CARTESIAN_POINT('Origin',(0.,2.5,12.));
#7747=CARTESIAN_POINT('',(2.99903459153175,2.5,13.2523144648194));
#7748=CARTESIAN_POINT('Origin',(0.,2.5,12.));
#7749=CARTESIAN_POINT('',(-1.2,2.5,12.));
#7750=CARTESIAN_POINT('Origin',(0.,2.5,12.));
#7751=CARTESIAN_POINT('',(-1.2,2.5,12.));
#7752=CARTESIAN_POINT('Origin',(0.,2.5,12.));
#7753=CARTESIAN_POINT('',(-2.60150387000671,2.5,10.0520067725117));
#7754=CARTESIAN_POINT('',(-2.60150387000671,2.5,10.0520067725117));
#7755=CARTESIAN_POINT('',(2.60150387000671,2.5,10.0520067725117));
#7756=CARTESIAN_POINT('Origin',(0.,2.5,12.));
#7757=CARTESIAN_POINT('',(2.60150387000671,2.5,10.0520067725117));
#7758=CARTESIAN_POINT('Origin',(-3.5,2.4,10.));
#7759=CARTESIAN_POINT('',(-4.4,2.5,10.));
#7760=CARTESIAN_POINT('Origin',(-3.5,2.5,10.));
#7761=CARTESIAN_POINT('',(-4.4,3.1,10.));
#7762=CARTESIAN_POINT('',(-4.4,2.4,10.));
#7763=CARTESIAN_POINT('Origin',(-3.5,3.1,10.));
#7764=CARTESIAN_POINT('Origin',(-3.5,2.5,10.));
#7765=CARTESIAN_POINT('Origin',(-3.5,2.4,14.));
#7766=CARTESIAN_POINT('',(-4.4,2.5,14.));
#7767=CARTESIAN_POINT('Origin',(-3.5,2.5,14.));
#7768=CARTESIAN_POINT('',(-4.4,3.1,14.));
#7769=CARTESIAN_POINT('',(-4.4,2.4,14.));
#7770=CARTESIAN_POINT('Origin',(-3.5,3.1,14.));
#7771=CARTESIAN_POINT('Origin',(-3.5,2.5,14.));
#7772=CARTESIAN_POINT('Origin',(0.,2.5,13.25));
#7773=CARTESIAN_POINT('',(-1.,2.5,12.));
#7774=CARTESIAN_POINT('Origin',(0.,2.5,12.));
#7775=CARTESIAN_POINT('Origin',(3.5,2.4,10.));
#7776=CARTESIAN_POINT('',(2.6,2.5,10.));
#7777=CARTESIAN_POINT('Origin',(3.5,2.5,10.));
#7778=CARTESIAN_POINT('',(2.6,3.1,10.));
#7779=CARTESIAN_POINT('',(2.6,2.4,10.));
#7780=CARTESIAN_POINT('Origin',(3.5,3.1,10.));
#7781=CARTESIAN_POINT('Origin',(3.5,2.5,10.));
#7782=CARTESIAN_POINT('Origin',(3.5,2.4,14.));
#7783=CARTESIAN_POINT('',(2.6,2.5,14.));
#7784=CARTESIAN_POINT('Origin',(3.5,2.5,14.));
#7785=CARTESIAN_POINT('',(2.6,3.1,14.));
#7786=CARTESIAN_POINT('',(2.6,2.4,14.));
#7787=CARTESIAN_POINT('Origin',(3.5,3.1,14.));
#7788=CARTESIAN_POINT('Origin',(3.5,2.5,14.));
#7789=CARTESIAN_POINT('Origin',(-2.,2.4,5.));
#7790=CARTESIAN_POINT('',(-2.425,2.5,5.));
#7791=CARTESIAN_POINT('Origin',(-2.,2.5,5.));
#7792=CARTESIAN_POINT('',(-2.425,3.1,5.));
#7793=CARTESIAN_POINT('',(-2.425,2.4,5.));
#7794=CARTESIAN_POINT('Origin',(-2.,3.1,5.));
#7795=CARTESIAN_POINT('Origin',(2.,2.4,5.));
#7796=CARTESIAN_POINT('',(1.575,2.5,5.));
#7797=CARTESIAN_POINT('Origin',(2.,2.5,5.));
#7798=CARTESIAN_POINT('',(1.575,3.1,5.));
#7799=CARTESIAN_POINT('',(1.575,2.4,5.));
#7800=CARTESIAN_POINT('Origin',(2.,3.1,5.));
#7801=CARTESIAN_POINT('Origin',(0.,2.4,20.5));
#7802=CARTESIAN_POINT('',(-0.425,2.5,20.5));
#7803=CARTESIAN_POINT('Origin',(0.,2.5,20.5));
#7804=CARTESIAN_POINT('',(-0.425,3.1,20.5));
#7805=CARTESIAN_POINT('',(-0.425,2.4,20.5));
#7806=CARTESIAN_POINT('Origin',(0.,3.1,20.5));
#7807=CARTESIAN_POINT('Origin',(0.,2.4,12.));
#7808=CARTESIAN_POINT('',(-1.,3.1,12.));
#7809=CARTESIAN_POINT('',(-1.,2.4,12.));
#7810=CARTESIAN_POINT('Origin',(0.,3.1,12.));
#7811=CARTESIAN_POINT('Origin',(-3.,2.5,4.5));
#7812=CARTESIAN_POINT('',(-6.,2.5,9.));
#7813=CARTESIAN_POINT('',(-3.,2.5,4.5));
#7814=CARTESIAN_POINT('',(-6.,2.5,9.));
#7815=CARTESIAN_POINT('',(-6.,3.1,9.));
#7816=CARTESIAN_POINT('',(-6.,2.5,9.));
#7817=CARTESIAN_POINT('',(-3.,3.1,4.5));
#7818=CARTESIAN_POINT('',(-6.,3.1,9.));
#7819=CARTESIAN_POINT('',(-3.,2.5,4.5));
#7820=CARTESIAN_POINT('Origin',(3.,2.5,4.5));
#7821=CARTESIAN_POINT('',(3.,2.5,4.5));
#7822=CARTESIAN_POINT('',(-3.,2.5,4.5));
#7823=CARTESIAN_POINT('',(3.,3.1,4.5));
#7824=CARTESIAN_POINT('',(-3.,3.1,4.5));
#7825=CARTESIAN_POINT('',(3.,2.5,4.5));
#7826=CARTESIAN_POINT('Origin',(6.,2.5,9.));
#7827=CARTESIAN_POINT('',(6.,2.5,9.));
#7828=CARTESIAN_POINT('',(3.,2.5,4.5));
#7829=CARTESIAN_POINT('',(6.,3.1,9.));
#7830=CARTESIAN_POINT('',(3.,3.1,4.5));
#7831=CARTESIAN_POINT('',(6.,2.5,9.));
#7832=CARTESIAN_POINT('Origin',(6.,2.5,15.));
#7833=CARTESIAN_POINT('',(6.,2.5,15.));
#7834=CARTESIAN_POINT('',(6.,2.5,9.));
#7835=CARTESIAN_POINT('',(6.,3.1,15.));
#7836=CARTESIAN_POINT('',(6.,3.1,9.));
#7837=CARTESIAN_POINT('',(6.,2.5,15.));
#7838=CARTESIAN_POINT('Origin',(2.5,2.5,22.));
#7839=CARTESIAN_POINT('',(2.5,2.5,22.));
#7840=CARTESIAN_POINT('',(6.,2.5,15.));
#7841=CARTESIAN_POINT('',(2.5,3.1,22.));
#7842=CARTESIAN_POINT('',(6.,3.1,15.));
#7843=CARTESIAN_POINT('',(2.5,2.5,22.));
#7844=CARTESIAN_POINT('Origin',(-2.5,2.5,22.));
#7845=CARTESIAN_POINT('',(-2.5,2.5,22.));
#7846=CARTESIAN_POINT('',(2.5,2.5,22.));
#7847=CARTESIAN_POINT('',(-2.5,3.1,22.));
#7848=CARTESIAN_POINT('',(2.5,3.1,22.));
#7849=CARTESIAN_POINT('',(-2.5,2.5,22.));
#7850=CARTESIAN_POINT('Origin',(-6.,2.5,15.));
#7851=CARTESIAN_POINT('',(-6.,2.5,15.));
#7852=CARTESIAN_POINT('',(-2.5,2.5,22.));
#7853=CARTESIAN_POINT('',(-6.,3.1,15.));
#7854=CARTESIAN_POINT('',(-2.5,3.1,22.));
#7855=CARTESIAN_POINT('',(-6.,2.5,15.));
#7856=CARTESIAN_POINT('Origin',(-6.,2.5,9.));
#7857=CARTESIAN_POINT('',(-6.,2.5,15.));
#7858=CARTESIAN_POINT('',(-6.,3.1,15.));
#7859=CARTESIAN_POINT('Origin',(0.,3.1,13.25));
#7860=CARTESIAN_POINT('Origin',(0.,2.5,13.25));
#7861=CARTESIAN_POINT('',(0.,0.,0.));
#7862=CARTESIAN_POINT('Origin',(0.,0.,4.4));
#7863=CARTESIAN_POINT('',(-1.1,-1.34711147906209E-16,4.5));
#7864=CARTESIAN_POINT('Origin',(0.,0.,4.5));
#7865=CARTESIAN_POINT('',(-1.1,1.34711147906209E-16,5.5));
#7866=CARTESIAN_POINT('',(-1.1,-1.34711147906209E-16,4.4));
#7867=CARTESIAN_POINT('Origin',(0.,0.,5.5));
#7868=CARTESIAN_POINT('Origin',(-2.,-2.6,5.));
#7869=CARTESIAN_POINT('',(-2.425,-2.5,5.));
#7870=CARTESIAN_POINT('Origin',(-2.,-2.5,5.));
#7871=CARTESIAN_POINT('',(-2.425,2.5,5.));
#7872=CARTESIAN_POINT('',(-2.425,-2.6,5.));
#7873=CARTESIAN_POINT('Origin',(-2.,2.5,5.));
#7874=CARTESIAN_POINT('Origin',(2.,-2.6,5.));
#7875=CARTESIAN_POINT('',(1.575,-2.5,5.));
#7876=CARTESIAN_POINT('Origin',(2.,-2.5,5.));
#7877=CARTESIAN_POINT('',(1.575,2.5,5.));
#7878=CARTESIAN_POINT('',(1.575,-2.6,5.));
#7879=CARTESIAN_POINT('Origin',(2.,2.5,5.));
#7880=CARTESIAN_POINT('Origin',(3.,2.5,4.5));
#7881=CARTESIAN_POINT('',(3.,2.5,4.5));
#7882=CARTESIAN_POINT('',(-3.,2.5,4.5));
#7883=CARTESIAN_POINT('',(3.,2.5,4.5));
#7884=CARTESIAN_POINT('',(-3.,2.5,5.5));
#7885=CARTESIAN_POINT('',(-3.,2.5,4.5));
#7886=CARTESIAN_POINT('',(3.,2.5,5.5));
#7887=CARTESIAN_POINT('',(3.,2.5,5.5));
#7888=CARTESIAN_POINT('',(3.,2.5,4.5));
#7889=CARTESIAN_POINT('Origin',(3.,-2.5,4.5));
#7890=CARTESIAN_POINT('',(3.,-2.5,4.5));
#7891=CARTESIAN_POINT('',(3.,-2.5,4.5));
#7892=CARTESIAN_POINT('',(3.,-2.5,5.5));
#7893=CARTESIAN_POINT('',(3.,-2.5,5.5));
#7894=CARTESIAN_POINT('',(3.,-2.5,4.5));
#7895=CARTESIAN_POINT('Origin',(-3.,-2.5,4.5));
#7896=CARTESIAN_POINT('',(-3.,-2.5,4.5));
#7897=CARTESIAN_POINT('',(-3.,-2.5,4.5));
#7898=CARTESIAN_POINT('',(-3.,-2.5,5.5));
#7899=CARTESIAN_POINT('',(-3.,-2.5,5.5));
#7900=CARTESIAN_POINT('',(-3.,-2.5,4.5));
#7901=CARTESIAN_POINT('Origin',(-3.,2.5,4.5));
#7902=CARTESIAN_POINT('',(-3.,2.5,4.5));
#7903=CARTESIAN_POINT('',(-3.,2.5,5.5));
#7904=CARTESIAN_POINT('Origin',(0.,0.,5.5));
#7905=CARTESIAN_POINT('Origin',(0.,0.,4.5));
#7906=CARTESIAN_POINT('',(0.,0.,0.));
#7907=CARTESIAN_POINT('Origin',(0.,-2.5,20.5));
#7908=CARTESIAN_POINT('',(-0.425,2.5,20.5));
#7909=CARTESIAN_POINT('Origin',(0.,2.5,20.5));
#7910=CARTESIAN_POINT('',(-0.425,-2.5,20.5));
#7911=CARTESIAN_POINT('',(-0.425,-2.5,20.5));
#7912=CARTESIAN_POINT('Origin',(0.,-2.5,20.5));
#7913=CARTESIAN_POINT('Origin',(0.,-2.5,20.5));
#7914=CARTESIAN_POINT('',(-1.,2.5,20.5));
#7915=CARTESIAN_POINT('Origin',(0.,2.5,20.5));
#7916=CARTESIAN_POINT('',(-1.,-2.5,20.5));
#7917=CARTESIAN_POINT('',(-1.,-2.5,20.5));
#7918=CARTESIAN_POINT('Origin',(0.,-2.5,20.5));
#7919=CARTESIAN_POINT('Origin',(0.,2.5,20.5));
#7920=CARTESIAN_POINT('Origin',(0.,-2.5,20.5));
#7921=CARTESIAN_POINT('',(0.,0.,0.));
#7922=CARTESIAN_POINT('Origin',(0.,0.3,12.));
#7923=CARTESIAN_POINT('',(-0.34,0.3,12.));
#7924=CARTESIAN_POINT('Origin',(0.,0.3,12.));
#7925=CARTESIAN_POINT('',(-0.34,3.1,12.));
#7926=CARTESIAN_POINT('',(-0.34,0.3,12.));
#7927=CARTESIAN_POINT('Origin',(0.,3.1,12.));
#7928=CARTESIAN_POINT('Origin',(0.,0.3,12.));
#7929=CARTESIAN_POINT('Origin',(0.,-3.1,12.));
#7930=CARTESIAN_POINT('',(-1.5,-3.1,12.));
#7931=CARTESIAN_POINT('Origin',(0.,-3.1,12.));
#7932=CARTESIAN_POINT('',(-1.,-3.1,12.));
#7933=CARTESIAN_POINT('Origin',(0.,-3.1,12.));
#7934=CARTESIAN_POINT('Origin',(0.,-3.5,12.));
#7935=CARTESIAN_POINT('',(-1.5,-3.5,12.));
#7936=CARTESIAN_POINT('',(-1.5,-3.5,12.));
#7937=CARTESIAN_POINT('Origin',(0.,-3.5,12.));
#7938=CARTESIAN_POINT('Origin',(0.,-3.5,12.));
#7939=CARTESIAN_POINT('Origin',(0.,-3.1,12.));
#7940=CARTESIAN_POINT('',(-1.,3.1,12.));
#7941=CARTESIAN_POINT('Origin',(0.,3.1,12.));
#7942=CARTESIAN_POINT('',(-1.,-3.1,12.));
#7943=CARTESIAN_POINT('Origin',(0.,3.1,12.));
#7944=CARTESIAN_POINT('',(0.,0.,0.));
#7945=CARTESIAN_POINT('Origin',(0.,3.1,12.));
#7946=CARTESIAN_POINT('',(-0.425,3.4,12.));
#7947=CARTESIAN_POINT('Origin',(0.,3.4,12.));
#7948=CARTESIAN_POINT('',(-0.425,3.1,12.));
#7949=CARTESIAN_POINT('',(-0.425,3.1,12.));
#7950=CARTESIAN_POINT('Origin',(0.,3.1,12.));
#7951=CARTESIAN_POINT('Origin',(0.,3.1,12.));
#7952=CARTESIAN_POINT('',(-1.5,3.4,12.));
#7953=CARTESIAN_POINT('Origin',(0.,3.4,12.));
#7954=CARTESIAN_POINT('',(-1.5,3.1,12.));
#7955=CARTESIAN_POINT('',(-1.5,3.1,12.));
#7956=CARTESIAN_POINT('Origin',(0.,3.1,12.));
#7957=CARTESIAN_POINT('Origin',(0.,3.4,12.));
#7958=CARTESIAN_POINT('Origin',(0.,3.1,12.));
#7959=CARTESIAN_POINT('',(0.,0.,0.));
#7960=CARTESIAN_POINT('Origin',(0.,-2.5,12.));
#7961=CARTESIAN_POINT('',(-1.005,-1.7,12.));
#7962=CARTESIAN_POINT('Origin',(0.,-1.7,12.));
#7963=CARTESIAN_POINT('',(-1.005,-2.5,12.));
#7964=CARTESIAN_POINT('',(-1.005,-2.5,12.));
#7965=CARTESIAN_POINT('Origin',(0.,-2.5,12.));
#7966=CARTESIAN_POINT('Origin',(0.,-2.5,12.));
#7967=CARTESIAN_POINT('',(-1.4,-1.7,12.));
#7968=CARTESIAN_POINT('Origin',(0.,-1.7,12.));
#7969=CARTESIAN_POINT('',(-1.4,-2.5,12.));
#7970=CARTESIAN_POINT('',(-1.4,-2.5,12.));
#7971=CARTESIAN_POINT('Origin',(0.,-2.5,12.));
#7972=CARTESIAN_POINT('Origin',(0.,-1.7,12.));
#7973=CARTESIAN_POINT('Origin',(0.,-2.5,12.));
#7974=CARTESIAN_POINT('',(0.,0.,0.));
#7975=CARTESIAN_POINT('Origin',(0.,1.7,12.));
#7976=CARTESIAN_POINT('',(-1.005,2.5,12.));
#7977=CARTESIAN_POINT('Origin',(0.,2.5,12.));
#7978=CARTESIAN_POINT('',(-1.005,1.7,12.));
#7979=CARTESIAN_POINT('',(-1.005,1.7,12.));
#7980=CARTESIAN_POINT('Origin',(0.,1.7,12.));
#7981=CARTESIAN_POINT('Origin',(0.,1.7,12.));
#7982=CARTESIAN_POINT('',(-1.4,2.5,12.));
#7983=CARTESIAN_POINT('Origin',(0.,2.5,12.));
#7984=CARTESIAN_POINT('',(-1.4,1.7,12.));
#7985=CARTESIAN_POINT('',(-1.4,1.7,12.));
#7986=CARTESIAN_POINT('Origin',(0.,1.7,12.));
#7987=CARTESIAN_POINT('Origin',(0.,2.5,12.));
#7988=CARTESIAN_POINT('Origin',(0.,1.7,12.));
#7989=CARTESIAN_POINT('',(0.,0.,0.));
#7990=CARTESIAN_POINT('Origin',(0.,-0.3,12.));
#7991=CARTESIAN_POINT('',(-1.005,0.3,12.));
#7992=CARTESIAN_POINT('Origin',(0.,0.3,12.));
#7993=CARTESIAN_POINT('',(-1.005,-0.3,12.));
#7994=CARTESIAN_POINT('',(-1.005,-0.3,12.));
#7995=CARTESIAN_POINT('Origin',(0.,-0.3,12.));
#7996=CARTESIAN_POINT('Origin',(0.,-0.3,12.));
#7997=CARTESIAN_POINT('',(-1.4,0.3,12.));
#7998=CARTESIAN_POINT('Origin',(0.,0.3,12.));
#7999=CARTESIAN_POINT('',(-1.4,-0.3,12.));
#8000=CARTESIAN_POINT('',(-1.4,-0.3,12.));
#8001=CARTESIAN_POINT('Origin',(0.,-0.3,12.));
#8002=CARTESIAN_POINT('Origin',(0.,0.3,12.));
#8003=CARTESIAN_POINT('Origin',(0.,-0.3,12.));
#8004=CARTESIAN_POINT('',(0.,0.,0.));
#8005=CARTESIAN_POINT('Origin',(0.,0.,4.5));
#8006=CARTESIAN_POINT('',(-0.81,-9.91963907309356E-17,5.5));
#8007=CARTESIAN_POINT('Origin',(0.,0.,5.5));
#8008=CARTESIAN_POINT('',(-0.81,-9.91963907309356E-17,4.5));
#8009=CARTESIAN_POINT('',(-0.81,-9.91963907309356E-17,4.5));
#8010=CARTESIAN_POINT('Origin',(0.,0.,4.5));
#8011=CARTESIAN_POINT('Origin',(0.,0.,4.5));
#8012=CARTESIAN_POINT('',(-1.1,-1.34711147906209E-16,5.5));
#8013=CARTESIAN_POINT('Origin',(0.,0.,5.5));
#8014=CARTESIAN_POINT('',(-1.1,-1.34711147906209E-16,4.5));
#8015=CARTESIAN_POINT('',(-1.1,-1.34711147906209E-16,4.5));
#8016=CARTESIAN_POINT('Origin',(0.,0.,4.5));
#8017=CARTESIAN_POINT('Origin',(0.,0.,5.5));
#8018=CARTESIAN_POINT('Origin',(0.,0.,4.5));
#8019=CARTESIAN_POINT('',(0.,0.,0.));
#8020=CARTESIAN_POINT('Origin',(0.,-2.5,20.5));
#8021=CARTESIAN_POINT('',(-1.005,-0.8,20.5));
#8022=CARTESIAN_POINT('Origin',(0.,-0.8,20.5));
#8023=CARTESIAN_POINT('',(-1.005,-2.5,20.5));
#8024=CARTESIAN_POINT('',(-1.005,-2.5,20.5));
#8025=CARTESIAN_POINT('Origin',(0.,-2.5,20.5));
#8026=CARTESIAN_POINT('Origin',(0.,-2.5,20.5));
#8027=CARTESIAN_POINT('',(-1.4,-0.8,20.5));
#8028=CARTESIAN_POINT('Origin',(0.,-0.8,20.5));
#8029=CARTESIAN_POINT('',(-1.4,-2.5,20.5));
#8030=CARTESIAN_POINT('',(-1.4,-2.5,20.5));
#8031=CARTESIAN_POINT('Origin',(0.,-2.5,20.5));
#8032=CARTESIAN_POINT('Origin',(0.,-0.8,20.5));
#8033=CARTESIAN_POINT('Origin',(0.,-2.5,20.5));
#8034=CARTESIAN_POINT('',(0.,0.,0.));
#8035=CARTESIAN_POINT('Origin',(0.,0.8,20.5));
#8036=CARTESIAN_POINT('',(-1.005,2.5,20.5));
#8037=CARTESIAN_POINT('Origin',(0.,2.5,20.5));
#8038=CARTESIAN_POINT('',(-1.005,0.8,20.5));
#8039=CARTESIAN_POINT('',(-1.005,0.8,20.5));
#8040=CARTESIAN_POINT('Origin',(0.,0.8,20.5));
#8041=CARTESIAN_POINT('Origin',(0.,0.8,20.5));
#8042=CARTESIAN_POINT('',(-1.4,2.5,20.5));
#8043=CARTESIAN_POINT('Origin',(0.,2.5,20.5));
#8044=CARTESIAN_POINT('',(-1.4,0.8,20.5));
#8045=CARTESIAN_POINT('',(-1.4,0.8,20.5));
#8046=CARTESIAN_POINT('Origin',(0.,0.8,20.5));
#8047=CARTESIAN_POINT('Origin',(0.,2.5,20.5));
#8048=CARTESIAN_POINT('Origin',(0.,0.8,20.5));
#8049=CARTESIAN_POINT('',(0.,0.,0.));
#8050=CARTESIAN_POINT('Origin',(0.173205080756888,-0.8,-0.3));
#8051=CARTESIAN_POINT('',(0.346410161513775,-0.8,0.));
#8052=CARTESIAN_POINT('',(0.173205080756888,-0.8,-0.3));
#8053=CARTESIAN_POINT('',(0.346410161513775,-0.8,0.));
#8054=CARTESIAN_POINT('',(0.173205080756888,-1.28,-0.3));
#8055=CARTESIAN_POINT('',(0.173205080756888,-0.8,-0.3));
#8056=CARTESIAN_POINT('',(0.346410161513775,-1.28,0.));
#8057=CARTESIAN_POINT('',(0.346410161513775,-1.28,0.));
#8058=CARTESIAN_POINT('',(0.346410161513775,-0.8,0.));
#8059=CARTESIAN_POINT('Origin',(-0.173205080756888,-0.8,-0.3));
#8060=CARTESIAN_POINT('',(-0.173205080756888,-0.8,-0.3));
#8061=CARTESIAN_POINT('',(0.173205080756888,-0.8,-0.3));
#8062=CARTESIAN_POINT('',(-0.173205080756888,-1.28,-0.3));
#8063=CARTESIAN_POINT('',(-0.173205080756888,-0.8,-0.3));
#8064=CARTESIAN_POINT('',(0.173205080756888,-1.28,-0.3));
#8065=CARTESIAN_POINT('Origin',(-0.346410161513775,-0.8,-5.55111512312578E-17));
#8066=CARTESIAN_POINT('',(-0.346410161513775,-0.8,-4.24230095489963E-17));
#8067=CARTESIAN_POINT('',(-0.173205080756888,-0.8,-0.3));
#8068=CARTESIAN_POINT('',(-0.346410161513775,-1.28,-5.55111512312578E-17));
#8069=CARTESIAN_POINT('',(-0.346410161513775,-0.8,-4.24230095489963E-17));
#8070=CARTESIAN_POINT('',(-0.173205080756888,-1.28,-0.3));
#8071=CARTESIAN_POINT('Origin',(-0.173205080756888,-0.8,0.3));
#8072=CARTESIAN_POINT('',(-0.173205080756888,-0.8,0.3));
#8073=CARTESIAN_POINT('',(-0.346410161513775,-0.8,-4.24230095489963E-17));
#8074=CARTESIAN_POINT('',(-0.173205080756888,-1.28,0.3));
#8075=CARTESIAN_POINT('',(-0.173205080756888,-0.8,0.3));
#8076=CARTESIAN_POINT('',(-0.346410161513775,-1.28,-4.24230095489963E-17));
#8077=CARTESIAN_POINT('Origin',(0.173205080756888,-0.8,0.3));
#8078=CARTESIAN_POINT('',(0.173205080756888,-0.8,0.3));
#8079=CARTESIAN_POINT('',(-0.173205080756888,-0.8,0.3));
#8080=CARTESIAN_POINT('',(0.173205080756888,-1.28,0.3));
#8081=CARTESIAN_POINT('',(0.173205080756888,-0.8,0.3));
#8082=CARTESIAN_POINT('',(-0.173205080756888,-1.28,0.3));
#8083=CARTESIAN_POINT('Origin',(0.346410161513775,-0.8,0.));
#8084=CARTESIAN_POINT('',(0.173205080756888,-0.8,0.3));
#8085=CARTESIAN_POINT('',(0.173205080756888,-1.28,0.3));
#8086=CARTESIAN_POINT('Origin',(0.,-0.8,-5.55111512312578E-17));
#8087=CARTESIAN_POINT('Origin',(0.,-1.28,-5.55111512312578E-17));
#8088=CARTESIAN_POINT('Origin',(0.,-2.9,0.));
#8089=CARTESIAN_POINT('',(-0.4,-2.9,4.89858719658941E-17));
#8090=CARTESIAN_POINT('Origin',(0.,-2.9,0.));
#8091=CARTESIAN_POINT('',(-0.3933,-2.9,4.81653586104654E-17));
#8092=CARTESIAN_POINT('Origin',(0.,-2.9,0.));
#8093=CARTESIAN_POINT('Origin',(0.,-7.5,0.));
#8094=CARTESIAN_POINT('',(-0.4,-7.5,4.89858719658941E-17));
#8095=CARTESIAN_POINT('',(-0.4,-7.5,4.89858719658941E-17));
#8096=CARTESIAN_POINT('Origin',(0.,-7.5,0.));
#8097=CARTESIAN_POINT('Origin',(0.,-7.5,0.));
#8098=CARTESIAN_POINT('Origin',(0.6,0.8,0.));
#8099=CARTESIAN_POINT('',(-0.6,0.8,-7.34788079488412E-17));
#8100=CARTESIAN_POINT('Origin',(0.,0.8,0.));
#8101=CARTESIAN_POINT('Origin',(0.,0.775,0.));
#8102=CARTESIAN_POINT('',(-0.65,0.75,-7.9602041944578E-17));
#8103=CARTESIAN_POINT('Origin',(0.,0.75,0.));
#8104=CARTESIAN_POINT('',(-0.625,0.775,-7.65404249467096E-17));
#8105=CARTESIAN_POINT('Origin',(0.,0.39,0.));
#8106=CARTESIAN_POINT('',(-0.65,0.0299999999999998,-7.9602041944578E-17));
#8107=CARTESIAN_POINT('Origin',(0.,0.0299999999999998,0.));
#8108=CARTESIAN_POINT('',(-0.65,0.39,-7.9602041944578E-17));
#8109=CARTESIAN_POINT('Origin',(0.,0.0150000000000001,0.));
#8110=CARTESIAN_POINT('',(-0.62,5.89805981832114E-17,-7.59281015471359E-17));
#8111=CARTESIAN_POINT('Origin',(0.,0.,0.));
#8112=CARTESIAN_POINT('',(-0.635,0.0150000000000001,-7.77650717458569E-17));
#8113=CARTESIAN_POINT('Origin',(0.42,0.,0.));
#8114=CARTESIAN_POINT('',(-0.42,-3.46944695195361E-18,-5.14351655641888E-17));
#8115=CARTESIAN_POINT('Origin',(0.,0.,0.));
#8116=CARTESIAN_POINT('Origin',(0.,-0.02,0.));
#8117=CARTESIAN_POINT('',(-0.3933,-0.0534000000000001,4.81653586104654E-17));
#8118=CARTESIAN_POINT('Origin',(0.,-0.0534000000000001,0.));
#8119=CARTESIAN_POINT('',(-0.41,-0.02,-5.02105187650415E-17));
#8120=CARTESIAN_POINT('Origin',(0.,-1.48,0.));
#8121=CARTESIAN_POINT('',(-0.3933,-1.48,-4.81653586104654E-17));
#8122=CARTESIAN_POINT('',(0.,0.,0.));
#8123=CARTESIAN_POINT('Origin',(0.,0.,0.));
#8124=CARTESIAN_POINT('',(-0.42,0.16,5.14351655641888E-17));
#8125=CARTESIAN_POINT('Origin',(0.,0.16,0.));
#8126=CARTESIAN_POINT('',(-0.42,0.,5.14351655641888E-17));
#8127=CARTESIAN_POINT('',(-0.42,0.,5.14351655641888E-17));
#8128=CARTESIAN_POINT('Origin',(0.,0.,0.));
#8129=CARTESIAN_POINT('Origin',(0.,0.,0.));
#8130=CARTESIAN_POINT('',(-0.8,0.16,9.79717439317883E-17));
#8131=CARTESIAN_POINT('Origin',(0.,0.16,0.));
#8132=CARTESIAN_POINT('',(-0.8,0.,9.79717439317883E-17));
#8133=CARTESIAN_POINT('',(-0.8,0.,9.79717439317883E-17));
#8134=CARTESIAN_POINT('Origin',(0.,0.,0.));
#8135=CARTESIAN_POINT('Origin',(0.,0.16,0.));
#8136=CARTESIAN_POINT('Origin',(0.,0.,0.));
#8137=CARTESIAN_POINT('',(0.,0.,0.));
#8138=CARTESIAN_POINT('Origin',(0.,0.067277284513851,0.));
#8139=CARTESIAN_POINT('',(-0.375277674973257,0.0768195421087395,0.65));
#8140=CARTESIAN_POINT('',(0.375277674973257,0.0768195421087395,0.65));
#8141=CARTESIAN_POINT('Ctrl Pts',(-0.375277674973257,0.0768195421087395,
0.65));
#8142=CARTESIAN_POINT('Ctrl Pts',(1.66533453693773E-13,-0.0315137912242439,
0.65));
#8143=CARTESIAN_POINT('Ctrl Pts',(0.375277674973257,0.0768195421087394,
0.65));
#8144=CARTESIAN_POINT('',(-0.750555349946514,0.0768195421087394,-9.19165206894919E-17));
#8145=CARTESIAN_POINT('Ctrl Pts',(-0.750555349946514,0.0768195421087394,
-9.19165206894919E-17));
#8146=CARTESIAN_POINT('Ctrl Pts',(-0.562916512459802,-0.0315137912242434,
0.325000000000144));
#8147=CARTESIAN_POINT('Ctrl Pts',(-0.375277674973257,0.0768195421087395,
0.65));
#8148=CARTESIAN_POINT('',(-0.6175,-2.77555756156289E-17,-7.5621939847349E-17));
#8149=CARTESIAN_POINT('',(-0.734027674973257,0.067277284513851,-8.98924642641573E-17));
#8150=CARTESIAN_POINT('Origin',(0.,0.,0.));
#8151=CARTESIAN_POINT('',(-0.375277674973257,0.0768195421087395,-0.65));
#8152=CARTESIAN_POINT('Ctrl Pts',(-0.375277674973257,0.0768195421087395,
-0.65));
#8153=CARTESIAN_POINT('Ctrl Pts',(-0.562916512459968,-0.0315137912242437,
-0.324999999999856));
#8154=CARTESIAN_POINT('Ctrl Pts',(-0.750555349946514,0.0768195421087395,
-9.19165206894919E-17));
#8155=CARTESIAN_POINT('',(0.375277674973257,0.0768195421087395,-0.65));
#8156=CARTESIAN_POINT('Ctrl Pts',(0.375277674973257,0.0768195421087395,
-0.65));
#8157=CARTESIAN_POINT('Ctrl Pts',(-1.66144875635155E-13,-0.0315137912242437,
-0.65));
#8158=CARTESIAN_POINT('Ctrl Pts',(-0.375277674973257,0.0768195421087395,
-0.65));
#8159=CARTESIAN_POINT('',(0.750555349946514,0.0768195421087394,0.));
#8160=CARTESIAN_POINT('Ctrl Pts',(0.750555349946514,0.0768195421087394,
0.));
#8161=CARTESIAN_POINT('Ctrl Pts',(0.562916512459802,-0.0315137912242436,
-0.325000000000144));
#8162=CARTESIAN_POINT('Ctrl Pts',(0.375277674973257,0.0768195421087395,
-0.65));
#8163=CARTESIAN_POINT('Ctrl Pts',(0.375277674973257,0.0768195421087394,
0.65));
#8164=CARTESIAN_POINT('Ctrl Pts',(0.562916512459968,-0.0315137912242439,
0.324999999999856));
#8165=CARTESIAN_POINT('Ctrl Pts',(0.750555349946514,0.0768195421087394,
0.));
#8166=CARTESIAN_POINT('Origin',(0.,0.612722715486149,0.));
#8167=CARTESIAN_POINT('',(-0.6175,0.68,-7.5621939847349E-17));
#8168=CARTESIAN_POINT('Origin',(0.,0.68,0.));
#8169=CARTESIAN_POINT('',(-0.750555349946514,0.603180457891261,-9.19165206894919E-17));
#8170=CARTESIAN_POINT('',(-0.734027674973257,0.612722715486149,-8.98924642641573E-17));
#8171=CARTESIAN_POINT('',(-0.375277674973257,0.603180457891261,0.65));
#8172=CARTESIAN_POINT('Ctrl Pts',(-0.375277674973257,0.603180457891261,
0.65));
#8173=CARTESIAN_POINT('Ctrl Pts',(-0.562916512459968,0.711513791224243,
0.324999999999856));
#8174=CARTESIAN_POINT('Ctrl Pts',(-0.750555349946514,0.603180457891261,
-9.19165206894919E-17));
#8175=CARTESIAN_POINT('',(0.375277674973257,0.603180457891261,0.65));
#8176=CARTESIAN_POINT('Ctrl Pts',(0.375277674973257,0.603180457891261,0.65));
#8177=CARTESIAN_POINT('Ctrl Pts',(-1.66755498298699E-13,0.711513791224244,
0.65));
#8178=CARTESIAN_POINT('Ctrl Pts',(-0.375277674973257,0.603180457891261,
0.65));
#8179=CARTESIAN_POINT('',(0.750555349946514,0.603180457891261,0.));
#8180=CARTESIAN_POINT('Ctrl Pts',(0.750555349946514,0.603180457891261,0.));
#8181=CARTESIAN_POINT('Ctrl Pts',(0.562916512459802,0.711513791224244,0.325000000000144));
#8182=CARTESIAN_POINT('Ctrl Pts',(0.375277674973257,0.603180457891261,0.65));
#8183=CARTESIAN_POINT('',(0.375277674973257,0.603180457891261,-0.65));
#8184=CARTESIAN_POINT('Ctrl Pts',(0.375277674973257,0.603180457891261,-0.65));
#8185=CARTESIAN_POINT('Ctrl Pts',(0.562916512459969,0.711513791224244,-0.324999999999856));
#8186=CARTESIAN_POINT('Ctrl Pts',(0.750555349946514,0.603180457891261,0.));
#8187=CARTESIAN_POINT('',(-0.375277674973257,0.603180457891261,-0.65));
#8188=CARTESIAN_POINT('Ctrl Pts',(-0.375277674973257,0.603180457891261,
-0.65));
#8189=CARTESIAN_POINT('Ctrl Pts',(1.66422431391311E-13,0.711513791224244,
-0.65));
#8190=CARTESIAN_POINT('Ctrl Pts',(0.375277674973257,0.603180457891261,-0.65));
#8191=CARTESIAN_POINT('Ctrl Pts',(-0.750555349946514,0.603180457891261,
-9.19165206894919E-17));
#8192=CARTESIAN_POINT('Ctrl Pts',(-0.562916512459802,0.711513791224244,
-0.325000000000144));
#8193=CARTESIAN_POINT('Ctrl Pts',(-0.375277674973257,0.603180457891261,
-0.65));
#8194=CARTESIAN_POINT('Origin',(0.375277674973257,0.,-0.65));
#8195=CARTESIAN_POINT('',(-0.375277674973257,0.,-0.65));
#8196=CARTESIAN_POINT('',(0.375277674973257,0.,-0.65));
#8197=CARTESIAN_POINT('Origin',(-0.375277674973257,0.,-0.65));
#8198=CARTESIAN_POINT('',(-0.750555349946514,0.,-9.19165206894919E-17));
#8199=CARTESIAN_POINT('Origin',(-0.750555349946514,0.,-9.19165206894919E-17));
#8200=CARTESIAN_POINT('',(-0.375277674973257,0.,0.65));
#8201=CARTESIAN_POINT('Origin',(0.,0.,0.));
#8202=CARTESIAN_POINT('',(-0.338975,0.68,4.15124648740974E-17));
#8203=CARTESIAN_POINT('Origin',(0.,0.68,0.));
#8204=CARTESIAN_POINT('',(-0.338975,0.,4.15124648740974E-17));
#8205=CARTESIAN_POINT('',(-0.338975,0.,4.15124648740974E-17));
#8206=CARTESIAN_POINT('Origin',(0.,0.,0.));
#8207=CARTESIAN_POINT('Origin',(-0.375277674973257,0.,0.65));
#8208=CARTESIAN_POINT('',(0.375277674973257,0.,0.65));
#8209=CARTESIAN_POINT('Origin',(0.750555349946514,0.,0.));
#8210=CARTESIAN_POINT('',(0.750555349946514,0.,0.));
#8211=CARTESIAN_POINT('Origin',(0.375277674973257,0.,0.65));
#8212=CARTESIAN_POINT('Origin',(0.,0.68,-1.11022302462516E-16));
#8213=CARTESIAN_POINT('Origin',(0.,0.,-1.11022302462516E-16));
#8214=CARTESIAN_POINT('',(0.,0.,0.));
#8215=CARTESIAN_POINT('Origin',(0.6,0.8,0.));
#8216=CARTESIAN_POINT('',(-0.6,0.8,-7.34788079488412E-17));
#8217=CARTESIAN_POINT('Origin',(0.,0.8,0.));
#8218=CARTESIAN_POINT('Origin',(0.,0.775,0.));
#8219=CARTESIAN_POINT('',(-0.65,0.75,-7.9602041944578E-17));
#8220=CARTESIAN_POINT('Origin',(0.,0.75,0.));
#8221=CARTESIAN_POINT('',(-0.625,0.775,-7.65404249467096E-17));
#8222=CARTESIAN_POINT('Origin',(0.,0.39,0.));
#8223=CARTESIAN_POINT('',(-0.65,0.0299999999999998,-7.9602041944578E-17));
#8224=CARTESIAN_POINT('Origin',(0.,0.0299999999999998,0.));
#8225=CARTESIAN_POINT('',(-0.65,0.39,-7.9602041944578E-17));
#8226=CARTESIAN_POINT('Origin',(0.,0.0150000000000001,0.));
#8227=CARTESIAN_POINT('',(-0.62,5.89805981832114E-17,-7.59281015471359E-17));
#8228=CARTESIAN_POINT('Origin',(0.,0.,0.));
#8229=CARTESIAN_POINT('',(-0.635,0.0150000000000001,-7.77650717458569E-17));
#8230=CARTESIAN_POINT('Origin',(0.42,0.,0.));
#8231=CARTESIAN_POINT('',(-0.42,-3.46944695195361E-18,-5.14351655641888E-17));
#8232=CARTESIAN_POINT('Origin',(0.,0.,0.));
#8233=CARTESIAN_POINT('Origin',(0.,-0.02,0.));
#8234=CARTESIAN_POINT('',(-0.3933,-0.0534000000000001,4.81653586104654E-17));
#8235=CARTESIAN_POINT('Origin',(0.,-0.0534000000000001,0.));
#8236=CARTESIAN_POINT('',(-0.41,-0.02,-5.02105187650415E-17));
#8237=CARTESIAN_POINT('Origin',(0.,-1.48,0.));
#8238=CARTESIAN_POINT('',(-0.3933,-2.9267,4.81653586104654E-17));
#8239=CARTESIAN_POINT('Origin',(0.,-2.9267,0.));
#8240=CARTESIAN_POINT('',(-0.3933,-1.48,-4.81653586104654E-17));
#8241=CARTESIAN_POINT('Origin',(0.,-2.96,0.));
#8242=CARTESIAN_POINT('',(-0.32,-3.,-3.91886975727153E-17));
#8243=CARTESIAN_POINT('Origin',(0.,-3.,0.));
#8244=CARTESIAN_POINT('',(-0.36,-2.96,-4.40872847693047E-17));
#8245=CARTESIAN_POINT('Origin',(0.,-3.,0.));
#8246=CARTESIAN_POINT('Origin',(0.173205080756888,-0.8,-0.3));
#8247=CARTESIAN_POINT('',(0.346410161513775,-0.8,0.));
#8248=CARTESIAN_POINT('',(0.173205080756888,-0.8,-0.3));
#8249=CARTESIAN_POINT('',(0.346410161513775,-0.8,0.));
#8250=CARTESIAN_POINT('',(0.173205080756888,-1.28,-0.3));
#8251=CARTESIAN_POINT('',(0.173205080756888,-0.8,-0.3));
#8252=CARTESIAN_POINT('',(0.346410161513775,-1.28,0.));
#8253=CARTESIAN_POINT('',(0.346410161513775,-1.28,0.));
#8254=CARTESIAN_POINT('',(0.346410161513775,-0.8,0.));
#8255=CARTESIAN_POINT('Origin',(-0.173205080756888,-0.8,-0.3));
#8256=CARTESIAN_POINT('',(-0.173205080756888,-0.8,-0.3));
#8257=CARTESIAN_POINT('',(0.173205080756888,-0.8,-0.3));
#8258=CARTESIAN_POINT('',(-0.173205080756888,-1.28,-0.3));
#8259=CARTESIAN_POINT('',(-0.173205080756888,-0.8,-0.3));
#8260=CARTESIAN_POINT('',(0.173205080756888,-1.28,-0.3));
#8261=CARTESIAN_POINT('Origin',(-0.346410161513775,-0.8,-5.55111512312578E-17));
#8262=CARTESIAN_POINT('',(-0.346410161513775,-0.8,-4.24230095489963E-17));
#8263=CARTESIAN_POINT('',(-0.173205080756888,-0.8,-0.3));
#8264=CARTESIAN_POINT('',(-0.346410161513775,-1.28,-5.55111512312578E-17));
#8265=CARTESIAN_POINT('',(-0.346410161513775,-0.8,-4.24230095489963E-17));
#8266=CARTESIAN_POINT('',(-0.173205080756888,-1.28,-0.3));
#8267=CARTESIAN_POINT('Origin',(-0.173205080756888,-0.8,0.3));
#8268=CARTESIAN_POINT('',(-0.173205080756888,-0.8,0.3));
#8269=CARTESIAN_POINT('',(-0.346410161513775,-0.8,-4.24230095489963E-17));
#8270=CARTESIAN_POINT('',(-0.173205080756888,-1.28,0.3));
#8271=CARTESIAN_POINT('',(-0.173205080756888,-0.8,0.3));
#8272=CARTESIAN_POINT('',(-0.346410161513775,-1.28,-4.24230095489963E-17));
#8273=CARTESIAN_POINT('Origin',(0.173205080756888,-0.8,0.3));
#8274=CARTESIAN_POINT('',(0.173205080756888,-0.8,0.3));
#8275=CARTESIAN_POINT('',(-0.173205080756888,-0.8,0.3));
#8276=CARTESIAN_POINT('',(0.173205080756888,-1.28,0.3));
#8277=CARTESIAN_POINT('',(0.173205080756888,-0.8,0.3));
#8278=CARTESIAN_POINT('',(-0.173205080756888,-1.28,0.3));
#8279=CARTESIAN_POINT('Origin',(0.346410161513775,-0.8,0.));
#8280=CARTESIAN_POINT('',(0.173205080756888,-0.8,0.3));
#8281=CARTESIAN_POINT('',(0.173205080756888,-1.28,0.3));
#8282=CARTESIAN_POINT('Origin',(0.,-0.8,-5.55111512312578E-17));
#8283=CARTESIAN_POINT('Origin',(0.,-1.28,-5.55111512312578E-17));
#8284=CARTESIAN_POINT('',(0.,0.,0.));
#8285=CARTESIAN_POINT('',(0.,0.,0.));
#8286=CARTESIAN_POINT('',(0.,0.,0.));
#8287=CARTESIAN_POINT('',(0.,0.,0.));
#8288=CARTESIAN_POINT('',(0.,0.,0.));
#8289=CARTESIAN_POINT('',(0.,0.,0.));
#8290=CARTESIAN_POINT('',(0.,0.,0.));
#8291=CARTESIAN_POINT('',(0.,0.,0.));
#8292=CARTESIAN_POINT('',(0.,0.,0.));
#8293=CARTESIAN_POINT('',(0.,0.,0.));
#8294=CARTESIAN_POINT('',(0.,0.,0.));
#8295=CARTESIAN_POINT('',(0.,0.,0.));
#8296=CARTESIAN_POINT('',(-2.,3.1,5.));
#8297=CARTESIAN_POINT('',(-2.,3.26,5.));
#8298=CARTESIAN_POINT('',(-2.,-3.26,5.));
#8299=CARTESIAN_POINT('',(-2.,-3.94,5.));
#8300=CARTESIAN_POINT('',(2.,3.1,5.));
#8301=CARTESIAN_POINT('',(2.,3.26,5.));
#8302=CARTESIAN_POINT('',(2.,-3.26,5.));
#8303=CARTESIAN_POINT('',(2.,-3.94,5.));
#8304=CARTESIAN_POINT('',(0.,3.1,20.5));
#8305=CARTESIAN_POINT('',(0.,3.26,20.5));
#8306=CARTESIAN_POINT('',(0.,-3.26,20.5));
#8307=CARTESIAN_POINT('',(0.,-3.94,20.5));
#8308=CARTESIAN_POINT('',(0.,3.4,12.));
#8309=CARTESIAN_POINT('',(0.,0.,0.));
#8310=CARTESIAN_POINT('',(0.,0.,0.));
#8311=CARTESIAN_POINT('Origin',(-1.90918830920368,-2.1,10.0908116907963));
#8312=CARTESIAN_POINT('',(-2.07418830920368,-2.,10.0908116907963));
#8313=CARTESIAN_POINT('Origin',(-1.90918830920368,-2.,10.0908116907963));
#8314=CARTESIAN_POINT('',(-2.07418830920368,2.,10.0908116907963));
#8315=CARTESIAN_POINT('',(-2.07418830920368,-2.1,10.0908116907963));
#8316=CARTESIAN_POINT('Origin',(-1.90918830920368,2.,10.0908116907963));
#8317=CARTESIAN_POINT('Origin',(-1.90918830920368,-2.1,13.9091883092037));
#8318=CARTESIAN_POINT('',(-2.07418830920368,-2.,13.9091883092037));
#8319=CARTESIAN_POINT('Origin',(-1.90918830920368,-2.,13.9091883092037));
#8320=CARTESIAN_POINT('',(-2.07418830920368,2.,13.9091883092037));
#8321=CARTESIAN_POINT('',(-2.07418830920368,-2.1,13.9091883092037));
#8322=CARTESIAN_POINT('Origin',(-1.90918830920368,2.,13.9091883092037));
#8323=CARTESIAN_POINT('Origin',(1.90918830920368,-2.1,13.9091883092037));
#8324=CARTESIAN_POINT('',(1.74418830920368,-2.,13.9091883092037));
#8325=CARTESIAN_POINT('Origin',(1.90918830920368,-2.,13.9091883092037));
#8326=CARTESIAN_POINT('',(1.74418830920368,2.,13.9091883092037));
#8327=CARTESIAN_POINT('',(1.74418830920368,-2.1,13.9091883092037));
#8328=CARTESIAN_POINT('Origin',(1.90918830920368,2.,13.9091883092037));
#8329=CARTESIAN_POINT('Origin',(1.90918830920368,-2.1,10.0908116907963));
#8330=CARTESIAN_POINT('',(1.74418830920368,-2.,10.0908116907963));
#8331=CARTESIAN_POINT('Origin',(1.90918830920368,-2.,10.0908116907963));
#8332=CARTESIAN_POINT('',(1.74418830920368,2.,10.0908116907963));
#8333=CARTESIAN_POINT('',(1.74418830920368,-2.1,10.0908116907963));
#8334=CARTESIAN_POINT('Origin',(1.90918830920368,2.,10.0908116907963));
#8335=CARTESIAN_POINT('Origin',(0.,-0.3,12.));
#8336=CARTESIAN_POINT('',(-4.4,4.44089209850063E-16,12.));
#8337=CARTESIAN_POINT('Origin',(0.,0.,12.));
#8338=CARTESIAN_POINT('',(-5.,-0.6,12.));
#8339=CARTESIAN_POINT('',(-4.7,-0.3,12.));
#8340=CARTESIAN_POINT('Origin',(0.,-0.6,12.));
#8341=CARTESIAN_POINT('Origin',(0.,0.3,12.));
#8342=CARTESIAN_POINT('',(-5.,0.6,12.));
#8343=CARTESIAN_POINT('Origin',(0.,0.6,12.));
#8344=CARTESIAN_POINT('',(-4.7,0.3,12.));
#8345=CARTESIAN_POINT('Origin',(0.,-1.2,12.));
#8346=CARTESIAN_POINT('',(-5.,1.2,12.));
#8347=CARTESIAN_POINT('Origin',(0.,1.2,12.));
#8348=CARTESIAN_POINT('',(-5.,-1.2,12.));
#8349=CARTESIAN_POINT('Origin',(0.,1.2,12.));
#8350=CARTESIAN_POINT('',(-3.,1.2,12.));
#8351=CARTESIAN_POINT('Origin',(0.,1.2,12.));
#8352=CARTESIAN_POINT('Origin',(0.,-1.2,12.));
#8353=CARTESIAN_POINT('',(-5.,-1.2,12.));
#8354=CARTESIAN_POINT('Origin',(0.,-1.2,12.));
#8355=CARTESIAN_POINT('',(-3.,-1.2,12.));
#8356=CARTESIAN_POINT('Origin',(0.,-1.2,12.));
#8357=CARTESIAN_POINT('Origin',(0.,-1.2,12.));
#8358=CARTESIAN_POINT('',(-5.,-1.2,12.));
#8359=CARTESIAN_POINT('Origin',(0.,-2.,12.));
#8360=CARTESIAN_POINT('',(-3.,-2.,12.));
#8361=CARTESIAN_POINT('',(-3.,-2.,12.));
#8362=CARTESIAN_POINT('Origin',(0.,-2.,12.));
#8363=CARTESIAN_POINT('Origin',(0.,-2.,12.));
#8364=CARTESIAN_POINT('',(-2.35,2.,12.));
#8365=CARTESIAN_POINT('Origin',(0.,2.,12.));
#8366=CARTESIAN_POINT('',(-2.35,-2.,12.));
#8367=CARTESIAN_POINT('',(-2.35,-2.,12.));
#8368=CARTESIAN_POINT('Origin',(0.,-2.,12.));
#8369=CARTESIAN_POINT('Origin',(0.,-2.,12.));
#8370=CARTESIAN_POINT('',(-3.,2.,12.));
#8371=CARTESIAN_POINT('Origin',(0.,2.,12.));
#8372=CARTESIAN_POINT('',(-3.,-2.,12.));
#8373=CARTESIAN_POINT('Origin',(0.,2.,12.));
#8374=CARTESIAN_POINT('Origin',(0.,-2.,12.));
#8375=CARTESIAN_POINT('',(0.,0.,0.));
#8376=CARTESIAN_POINT('Origin',(0.,-0.3,12.));
#8377=CARTESIAN_POINT('',(-1.9,0.3,12.));
#8378=CARTESIAN_POINT('Origin',(0.,0.3,12.));
#8379=CARTESIAN_POINT('',(-1.9,-0.3,12.));
#8380=CARTESIAN_POINT('',(-1.9,-0.3,12.));
#8381=CARTESIAN_POINT('Origin',(0.,-0.3,12.));
#8382=CARTESIAN_POINT('Origin',(0.,-0.3,12.));
#8383=CARTESIAN_POINT('',(-2.34,0.3,12.));
#8384=CARTESIAN_POINT('Origin',(0.,0.3,12.));
#8385=CARTESIAN_POINT('',(-2.34,-0.3,12.));
#8386=CARTESIAN_POINT('',(-2.34,-0.3,12.));
#8387=CARTESIAN_POINT('Origin',(0.,-0.3,12.));
#8388=CARTESIAN_POINT('Origin',(0.,0.3,12.));
#8389=CARTESIAN_POINT('Origin',(0.,-0.3,12.));
#8390=CARTESIAN_POINT('',(0.,0.,0.));
#8391=CARTESIAN_POINT('Origin',(-1.90918830920368,-2.4,10.0908116907963));
#8392=CARTESIAN_POINT('',(-2.13418830920368,-2.3,10.0908116907963));
#8393=CARTESIAN_POINT('Origin',(-1.90918830920368,-2.3,10.0908116907963));
#8394=CARTESIAN_POINT('',(-2.13418830920368,-2.,10.0908116907963));
#8395=CARTESIAN_POINT('',(-2.13418830920368,-2.4,10.0908116907963));
#8396=CARTESIAN_POINT('Origin',(-1.90918830920368,-2.,10.0908116907963));
#8397=CARTESIAN_POINT('Origin',(-1.90918830920368,-2.4,13.9091883092037));
#8398=CARTESIAN_POINT('',(-2.13418830920368,-2.3,13.9091883092037));
#8399=CARTESIAN_POINT('Origin',(-1.90918830920368,-2.3,13.9091883092037));
#8400=CARTESIAN_POINT('',(-2.13418830920368,-2.,13.9091883092037));
#8401=CARTESIAN_POINT('',(-2.13418830920368,-2.4,13.9091883092037));
#8402=CARTESIAN_POINT('Origin',(-1.90918830920368,-2.,13.9091883092037));
#8403=CARTESIAN_POINT('Origin',(1.90918830920368,-2.4,13.9091883092037));
#8404=CARTESIAN_POINT('',(1.68418830920368,-2.3,13.9091883092037));
#8405=CARTESIAN_POINT('Origin',(1.90918830920368,-2.3,13.9091883092037));
#8406=CARTESIAN_POINT('',(1.68418830920368,-2.,13.9091883092037));
#8407=CARTESIAN_POINT('',(1.68418830920368,-2.4,13.9091883092037));
#8408=CARTESIAN_POINT('Origin',(1.90918830920368,-2.,13.9091883092037));
#8409=CARTESIAN_POINT('Origin',(1.90918830920368,-2.4,10.0908116907963));
#8410=CARTESIAN_POINT('',(1.68418830920368,-2.3,10.0908116907963));
#8411=CARTESIAN_POINT('Origin',(1.90918830920368,-2.3,10.0908116907963));
#8412=CARTESIAN_POINT('',(1.68418830920368,-2.,10.0908116907963));
#8413=CARTESIAN_POINT('',(1.68418830920368,-2.4,10.0908116907963));
#8414=CARTESIAN_POINT('Origin',(1.90918830920368,-2.,10.0908116907963));
#8415=CARTESIAN_POINT('Origin',(0.,-2.,12.));
#8416=CARTESIAN_POINT('',(-2.34,-1.7,12.));
#8417=CARTESIAN_POINT('Origin',(0.,-1.7,12.));
#8418=CARTESIAN_POINT('',(-2.34,-2.,12.));
#8419=CARTESIAN_POINT('',(-2.34,-2.,12.));
#8420=CARTESIAN_POINT('Origin',(0.,-2.,12.));
#8421=CARTESIAN_POINT('Origin',(0.,-1.7,12.));
#8422=CARTESIAN_POINT('',(-1.9,-1.7,12.));
#8423=CARTESIAN_POINT('Origin',(0.,-1.7,12.));
#8424=CARTESIAN_POINT('Origin',(0.,-2.3,12.));
#8425=CARTESIAN_POINT('',(-1.9,-2.3,12.));
#8426=CARTESIAN_POINT('',(-1.9,-2.3,12.));
#8427=CARTESIAN_POINT('Origin',(0.,-2.3,12.));
#8428=CARTESIAN_POINT('Origin',(0.,-2.3,12.));
#8429=CARTESIAN_POINT('',(-3.,-2.,12.));
#8430=CARTESIAN_POINT('Origin',(0.,-2.,12.));
#8431=CARTESIAN_POINT('',(-3.,-2.3,12.));
#8432=CARTESIAN_POINT('',(-3.,-2.3,12.));
#8433=CARTESIAN_POINT('Origin',(0.,-2.3,12.));
#8434=CARTESIAN_POINT('Origin',(0.,-2.,12.));
#8435=CARTESIAN_POINT('Origin',(0.,-2.3,12.));
#8436=CARTESIAN_POINT('',(0.,0.,0.));
#8437=CARTESIAN_POINT('Origin',(-1.90918830920368,1.9,10.0908116907963));
#8438=CARTESIAN_POINT('',(-2.13418830920368,2.,10.0908116907963));
#8439=CARTESIAN_POINT('Origin',(-1.90918830920368,2.,10.0908116907963));
#8440=CARTESIAN_POINT('',(-2.13418830920368,2.3,10.0908116907963));
#8441=CARTESIAN_POINT('',(-2.13418830920368,1.9,10.0908116907963));
#8442=CARTESIAN_POINT('Origin',(-1.90918830920368,2.3,10.0908116907963));
#8443=CARTESIAN_POINT('Origin',(-1.90918830920368,1.9,13.9091883092037));
#8444=CARTESIAN_POINT('',(-2.13418830920368,2.,13.9091883092037));
#8445=CARTESIAN_POINT('Origin',(-1.90918830920368,2.,13.9091883092037));
#8446=CARTESIAN_POINT('',(-2.13418830920368,2.3,13.9091883092037));
#8447=CARTESIAN_POINT('',(-2.13418830920368,1.9,13.9091883092037));
#8448=CARTESIAN_POINT('Origin',(-1.90918830920368,2.3,13.9091883092037));
#8449=CARTESIAN_POINT('Origin',(1.90918830920368,1.9,13.9091883092037));
#8450=CARTESIAN_POINT('',(1.68418830920368,2.,13.9091883092037));
#8451=CARTESIAN_POINT('Origin',(1.90918830920368,2.,13.9091883092037));
#8452=CARTESIAN_POINT('',(1.68418830920368,2.3,13.9091883092037));
#8453=CARTESIAN_POINT('',(1.68418830920368,1.9,13.9091883092037));
#8454=CARTESIAN_POINT('Origin',(1.90918830920368,2.3,13.9091883092037));
#8455=CARTESIAN_POINT('Origin',(1.90918830920368,1.9,10.0908116907963));
#8456=CARTESIAN_POINT('',(1.68418830920368,2.,10.0908116907963));
#8457=CARTESIAN_POINT('Origin',(1.90918830920368,2.,10.0908116907963));
#8458=CARTESIAN_POINT('',(1.68418830920368,2.3,10.0908116907963));
#8459=CARTESIAN_POINT('',(1.68418830920368,1.9,10.0908116907963));
#8460=CARTESIAN_POINT('Origin',(1.90918830920368,2.3,10.0908116907963));
#8461=CARTESIAN_POINT('Origin',(0.,1.7,12.));
#8462=CARTESIAN_POINT('',(-2.34,2.,12.));
#8463=CARTESIAN_POINT('Origin',(0.,2.,12.));
#8464=CARTESIAN_POINT('',(-2.34,1.7,12.));
#8465=CARTESIAN_POINT('',(-2.34,1.7,12.));
#8466=CARTESIAN_POINT('Origin',(0.,1.7,12.));
#8467=CARTESIAN_POINT('Origin',(0.,1.7,12.));
#8468=CARTESIAN_POINT('',(-1.9,1.7,12.));
#8469=CARTESIAN_POINT('Origin',(0.,1.7,12.));
#8470=CARTESIAN_POINT('Origin',(0.,2.,12.));
#8471=CARTESIAN_POINT('',(-1.9,2.3,12.));
#8472=CARTESIAN_POINT('Origin',(0.,2.3,12.));
#8473=CARTESIAN_POINT('',(-1.9,2.,12.));
#8474=CARTESIAN_POINT('Origin',(0.,2.,12.));
#8475=CARTESIAN_POINT('',(-3.,2.3,12.));
#8476=CARTESIAN_POINT('Origin',(0.,2.3,12.));
#8477=CARTESIAN_POINT('',(-3.,2.,12.));
#8478=CARTESIAN_POINT('',(-3.,2.,12.));
#8479=CARTESIAN_POINT('Origin',(0.,2.,12.));
#8480=CARTESIAN_POINT('Origin',(0.,2.3,12.));
#8481=CARTESIAN_POINT('Origin',(0.,2.,12.));
#8482=CARTESIAN_POINT('',(0.,0.,0.));
#8483=CARTESIAN_POINT('',(0.,0.,0.));
#8484=CARTESIAN_POINT('Origin',(0.,0.,0.));
#8485=CARTESIAN_POINT('',(-1.63531,-0.410863395882378,-2.00267715711366E-16));
#8486=CARTESIAN_POINT('',(-2.00267715711366E-16,-0.410863395882378,1.63531));
#8487=CARTESIAN_POINT('Origin',(0.,-0.410863395882378,0.));
#8488=CARTESIAN_POINT('Origin',(0.,-0.410863395882378,0.));
#8489=CARTESIAN_POINT('',(-2.00267715711366E-16,0.410863395882378,1.63531));
#8490=CARTESIAN_POINT('Origin',(-2.05128338857182E-16,0.,1.675));
#8491=CARTESIAN_POINT('',(-1.63531,0.410863395882378,2.00267715711366E-16));
#8492=CARTESIAN_POINT('Origin',(0.,0.410863395882378,0.));
#8493=CARTESIAN_POINT('Origin',(0.,0.410863395882378,0.));
#8494=CARTESIAN_POINT('Origin',(0.,0.,0.));
#8495=CARTESIAN_POINT('',(-1.63531,0.7,-2.00267715711366E-16));
#8496=CARTESIAN_POINT('',(-1.63531,0.,-2.00267715711366E-16));
#8497=CARTESIAN_POINT('Origin',(0.,0.7,0.));
#8498=CARTESIAN_POINT('Origin',(0.,0.,0.));
#8499=CARTESIAN_POINT('',(-1.,-0.6,-1.22464679914735E-16));
#8500=CARTESIAN_POINT('Origin',(0.,-0.6,0.));
#8501=CARTESIAN_POINT('',(-1.,0.6,-1.22464679914735E-16));
#8502=CARTESIAN_POINT('',(-1.,0.,-1.22464679914735E-16));
#8503=CARTESIAN_POINT('Origin',(0.,0.6,0.));
#8504=CARTESIAN_POINT('Origin',(0.,0.65,0.));
#8505=CARTESIAN_POINT('',(-1.1,0.7,-1.34711147906209E-16));
#8506=CARTESIAN_POINT('',(-1.05,0.65,-1.28587913910472E-16));
#8507=CARTESIAN_POINT('Origin',(0.,0.7,0.));
#8508=CARTESIAN_POINT('Origin',(1.63531,0.7,0.));
#8509=CARTESIAN_POINT('Origin',(0.,0.,0.));
#8510=CARTESIAN_POINT('',(-1.63531,-0.7,-2.00267715711366E-16));
#8511=CARTESIAN_POINT('Origin',(0.,-0.7,0.));
#8512=CARTESIAN_POINT('',(-1.63531,0.,-2.00267715711366E-16));
#8513=CARTESIAN_POINT('Origin',(1.1,-0.7,0.));
#8514=CARTESIAN_POINT('',(-1.1,-0.7,-1.34711147906209E-16));
#8515=CARTESIAN_POINT('Origin',(0.,-0.7,0.));
#8516=CARTESIAN_POINT('Origin',(0.,-0.65,0.));
#8517=CARTESIAN_POINT('',(-1.05,-0.65,-1.28587913910472E-16));
#8518=CARTESIAN_POINT('',(0.,0.,0.));
#8519=CARTESIAN_POINT('Origin',(0.,0.,0.));
#8520=CARTESIAN_POINT('',(-1.71469,0.410863395882378,-2.09988962002998E-16));
#8521=CARTESIAN_POINT('',(-2.09988962002998E-16,0.410863395882378,1.71469));
#8522=CARTESIAN_POINT('Origin',(0.,0.410863395882378,0.));
#8523=CARTESIAN_POINT('Origin',(0.,0.410863395882378,0.));
#8524=CARTESIAN_POINT('',(-2.09988962002998E-16,-0.410863395882378,1.71469));
#8525=CARTESIAN_POINT('Origin',(-2.05128338857182E-16,0.,1.675));
#8526=CARTESIAN_POINT('',(-1.71469,-0.410863395882378,2.09988962002998E-16));
#8527=CARTESIAN_POINT('Origin',(0.,-0.410863395882378,0.));
#8528=CARTESIAN_POINT('Origin',(0.,-0.410863395882378,0.));
#8529=CARTESIAN_POINT('Origin',(0.,0.,0.));
#8530=CARTESIAN_POINT('',(-1.71469,-0.7,-2.09988962002998E-16));
#8531=CARTESIAN_POINT('Origin',(0.,-0.7,0.));
#8532=CARTESIAN_POINT('',(-1.71469,0.,-2.09988962002998E-16));
#8533=CARTESIAN_POINT('Origin',(2.25,0.7,0.));
#8534=CARTESIAN_POINT('',(-2.25,0.7,-2.75545529808154E-16));
#8535=CARTESIAN_POINT('Origin',(0.,0.7,0.));
#8536=CARTESIAN_POINT('',(-1.71469,0.7,-2.09988962002998E-16));
#8537=CARTESIAN_POINT('Origin',(0.,0.7,0.));
#8538=CARTESIAN_POINT('Origin',(0.,0.65,0.));
#8539=CARTESIAN_POINT('',(-2.35,0.6,-2.87791997799628E-16));
#8540=CARTESIAN_POINT('Origin',(0.,0.6,0.));
#8541=CARTESIAN_POINT('',(-2.3,0.65,-2.81668763803891E-16));
#8542=CARTESIAN_POINT('Origin',(0.,0.,0.));
#8543=CARTESIAN_POINT('',(-2.35,-0.6,-2.87791997799628E-16));
#8544=CARTESIAN_POINT('Origin',(0.,-0.6,0.));
#8545=CARTESIAN_POINT('',(-2.35,0.,-2.87791997799628E-16));
#8546=CARTESIAN_POINT('Origin',(0.,-0.65,0.));
#8547=CARTESIAN_POINT('',(-2.25,-0.7,-2.75545529808154E-16));
#8548=CARTESIAN_POINT('Origin',(0.,-0.7,0.));
#8549=CARTESIAN_POINT('',(-2.3,-0.65,-2.81668763803891E-16));
#8550=CARTESIAN_POINT('Origin',(1.71469,-0.7,0.));
#8551=CARTESIAN_POINT('Origin',(0.,0.,0.));
#8552=CARTESIAN_POINT('',(-1.71469,0.,-2.09988962002998E-16));
#8553=CARTESIAN_POINT('',(0.,0.,0.));
#8554=CARTESIAN_POINT('Origin',(1.675,0.,0.));
#8555=CARTESIAN_POINT('',(1.675,-2.97627328869245E-33,0.3969));
#8556=CARTESIAN_POINT('',(1.675,-2.97627328869245E-33,-0.3969));
#8557=CARTESIAN_POINT('Origin',(1.675,0.,0.));
#8558=CARTESIAN_POINT('Origin',(1.18440385848747,0.,-1.18440385848747));
#8559=CARTESIAN_POINT('',(1.46505453994041,3.1867025333467E-33,-0.903753177034526));
#8560=CARTESIAN_POINT('',(0.903753177034527,-9.13924911073161E-33,-1.46505453994041));
#8561=CARTESIAN_POINT('Origin',(1.18440385848747,0.,-1.18440385848747));
#8562=CARTESIAN_POINT('Origin',(1.02564169428591E-16,0.,-1.675));
#8563=CARTESIAN_POINT('',(0.3969,-2.97627328869246E-33,-1.675));
#8564=CARTESIAN_POINT('',(-0.3969,-2.97627328869245E-33,-1.675));
#8565=CARTESIAN_POINT('Origin',(1.02564169428591E-16,0.,-1.675));
#8566=CARTESIAN_POINT('Origin',(-1.18440385848747,0.,-1.18440385848747));
#8567=CARTESIAN_POINT('',(-0.903753177034526,3.1867025333467E-33,-1.46505453994041));
#8568=CARTESIAN_POINT('',(-1.46505453994041,-9.13924911073161E-33,-0.903753177034527));
#8569=CARTESIAN_POINT('Origin',(-1.18440385848747,0.,-1.18440385848747));
#8570=CARTESIAN_POINT('Origin',(-1.675,0.,-2.05128338857182E-16));
#8571=CARTESIAN_POINT('',(-1.675,-2.97627328869246E-33,-0.3969));
#8572=CARTESIAN_POINT('',(-1.675,-2.97627328869245E-33,0.3969));
#8573=CARTESIAN_POINT('Origin',(-1.675,0.,-2.05128338857182E-16));
#8574=CARTESIAN_POINT('Origin',(-1.18440385848747,0.,1.18440385848747));
#8575=CARTESIAN_POINT('',(-1.46505453994041,6.26819044436628E-33,0.903753177034526));
#8576=CARTESIAN_POINT('',(-0.903753177034527,-1.22207370217512E-32,1.46505453994041));
#8577=CARTESIAN_POINT('Origin',(-1.18440385848747,0.,1.18440385848747));
#8578=CARTESIAN_POINT('Origin',(-3.07692508285772E-16,0.,1.675));
#8579=CARTESIAN_POINT('',(-0.3969,-2.97627328869246E-33,1.675));
#8580=CARTESIAN_POINT('',(0.396899999999999,-2.97627328869245E-33,1.675));
#8581=CARTESIAN_POINT('Origin',(-3.07692508285772E-16,0.,1.675));
#8582=CARTESIAN_POINT('Origin',(1.18440385848747,0.,1.18440385848747));
#8583=CARTESIAN_POINT('',(0.903753177034526,9.34967835538585E-33,1.46505453994041));
#8584=CARTESIAN_POINT('',(1.46505453994041,-1.53022249327708E-32,0.903753177034527));
#8585=CARTESIAN_POINT('Origin',(1.18440385848747,0.,1.18440385848747));
#8586=CARTESIAN_POINT('',(0.,0.,0.));
#8587=CARTESIAN_POINT('Origin',(1.18440385848747,0.,1.18440385848747));
#8588=CARTESIAN_POINT('',(0.846804978391753,-0.07938,1.40825612658882));
#8589=CARTESIAN_POINT('',(1.40825612658882,-0.07938,0.846804978391754));
#8590=CARTESIAN_POINT('Ctrl Pts',(0.846804978391752,-0.0793800000000001,
1.40825612658882));
#8591=CARTESIAN_POINT('Ctrl Pts',(0.854205272175554,-0.123401821157026,
1.40380622184538));
#8592=CARTESIAN_POINT('Ctrl Pts',(0.867957148219441,-0.166543350814306,
1.39550172959303));
#8593=CARTESIAN_POINT('Ctrl Pts',(0.902193646979982,-0.237231147975234,
1.3735491215176));
#8594=CARTESIAN_POINT('Ctrl Pts',(0.920778333482564,-0.266264900654909,
1.36127834356734));
#8595=CARTESIAN_POINT('Ctrl Pts',(0.962485392528369,-0.317195968905306,
1.33211611256184));
#8596=CARTESIAN_POINT('Ctrl Pts',(0.985600426557816,-0.33909093068465,1.31521005565926));
#8597=CARTESIAN_POINT('Ctrl Pts',(1.03253285680459,-0.373586846396559,1.27866649102984));
#8598=CARTESIAN_POINT('Ctrl Pts',(1.05871835910697,-0.388086240756494,1.25722555095714));
#8599=CARTESIAN_POINT('Ctrl Pts',(1.11153475808518,-0.407068917407805,1.2107812086231));
#8600=CARTESIAN_POINT('Ctrl Pts',(1.13814686046673,-0.411552957311693,1.18575674747573));
#8601=CARTESIAN_POINT('Ctrl Pts',(1.18575674747573,-0.411552957311693,1.13814686046673));
#8602=CARTESIAN_POINT('Ctrl Pts',(1.2107812086231,-0.407068917407805,1.11153475808518));
#8603=CARTESIAN_POINT('Ctrl Pts',(1.25722555095713,-0.388086240756494,1.05871835910697));
#8604=CARTESIAN_POINT('Ctrl Pts',(1.27866649102984,-0.373586846396559,1.03253285680459));
#8605=CARTESIAN_POINT('Ctrl Pts',(1.31521005565926,-0.33909093068465,0.985600426557816));
#8606=CARTESIAN_POINT('Ctrl Pts',(1.33211611256184,-0.317195968905306,0.962485392528369));
#8607=CARTESIAN_POINT('Ctrl Pts',(1.36127834356734,-0.266264900654909,0.920778333482565));
#8608=CARTESIAN_POINT('Ctrl Pts',(1.3735491215176,-0.237231147975234,0.902193646979983));
#8609=CARTESIAN_POINT('Ctrl Pts',(1.39550172959303,-0.166543350814306,0.867957148219442));
#8610=CARTESIAN_POINT('Ctrl Pts',(1.40380622184538,-0.123401821157026,0.854205272175555));
#8611=CARTESIAN_POINT('Ctrl Pts',(1.40825612658882,-0.0793800000000001,
0.846804978391753));
#8612=CARTESIAN_POINT('',(0.886256117232623,-0.07938,1.45861320581289));
#8613=CARTESIAN_POINT('Origin',(1.18440385848747,-0.07938,1.18440385848747));
#8614=CARTESIAN_POINT('',(1.45861320581289,-0.07938,0.886256117232624));
#8615=CARTESIAN_POINT('Ctrl Pts',(1.45861320581289,-0.0793800000000001,
0.886256117232623));
#8616=CARTESIAN_POINT('Ctrl Pts',(1.45630208793976,-0.101649918886749,0.890059788636852));
#8617=CARTESIAN_POINT('Ctrl Pts',(1.45296717977858,-0.123823518623746,0.895520212222107));
#8618=CARTESIAN_POINT('Ctrl Pts',(1.43904931717599,-0.192480977588836,0.917859913453975));
#8619=CARTESIAN_POINT('Ctrl Pts',(1.4243271592157,-0.236152929235938,0.940896403863072));
#8620=CARTESIAN_POINT('Ctrl Pts',(1.39055359345152,-0.303141259068212,0.990027513266106));
#8621=CARTESIAN_POINT('Ctrl Pts',(1.36743459453896,-0.335108247315849,1.02199477007745));
#8622=CARTESIAN_POINT('Ctrl Pts',(1.32643091652006,-0.373243761060364,1.07446535104584));
#8623=CARTESIAN_POINT('Ctrl Pts',(1.30441816675528,-0.387888272594439,1.10126842659597));
#8624=CARTESIAN_POINT('Ctrl Pts',(1.25681160160691,-0.407041111792943,1.15530234155453));
#8625=CARTESIAN_POINT('Ctrl Pts',(1.23119764287622,-0.411552957311693,1.18251418313119));
#8626=CARTESIAN_POINT('Ctrl Pts',(1.18251418313119,-0.411552957311693,1.23119764287622));
#8627=CARTESIAN_POINT('Ctrl Pts',(1.15530234155453,-0.407041111792943,1.25681160160691));
#8628=CARTESIAN_POINT('Ctrl Pts',(1.10126842659597,-0.387888272594439,1.30441816675528));
#8629=CARTESIAN_POINT('Ctrl Pts',(1.07446535104584,-0.373243761060364,1.32643091652006));
#8630=CARTESIAN_POINT('Ctrl Pts',(1.02199477007745,-0.335108247315848,1.36743459453896));
#8631=CARTESIAN_POINT('Ctrl Pts',(0.990027513266105,-0.303141259068211,
1.39055359345152));
#8632=CARTESIAN_POINT('Ctrl Pts',(0.940896403863071,-0.236152929235937,
1.42432715921571));
#8633=CARTESIAN_POINT('Ctrl Pts',(0.917859913453974,-0.192480977588835,
1.43904931717599));
#8634=CARTESIAN_POINT('Ctrl Pts',(0.895520212222106,-0.123823518623745,
1.45296717977858));
#8635=CARTESIAN_POINT('Ctrl Pts',(0.890059788636851,-0.101649918886749,
1.45630208793976));
#8636=CARTESIAN_POINT('Ctrl Pts',(0.886256117232622,-0.0793800000000001,
1.45861320581289));
#8637=CARTESIAN_POINT('Origin',(1.18440385848747,-0.07938,1.18440385848747));
#8638=CARTESIAN_POINT('Origin',(0.,-0.27783,0.));
#8639=CARTESIAN_POINT('',(0.404717578595295,-0.07938,1.65807299932179));
#8640=CARTESIAN_POINT('Origin',(0.,-0.07938,0.));
#8641=CARTESIAN_POINT('',(-0.404717578595296,-0.07938,1.65807299932179));
#8642=CARTESIAN_POINT('Ctrl Pts',(0.404717578595296,-0.0793800000000001,
1.65807299932179));
#8643=CARTESIAN_POINT('Ctrl Pts',(0.400393769631747,-0.101649918886749,
1.65912839404491));
#8644=CARTESIAN_POINT('Ctrl Pts',(0.394174530911058,-0.123823518623745,
1.66063136041479));
#8645=CARTESIAN_POINT('Ctrl Pts',(0.368536561654407,-0.192480977588835,
1.66658649961961));
#8646=CARTESIAN_POINT('Ctrl Pts',(0.341837165343982,-0.236152929235937,
1.67246562047521));
#8647=CARTESIAN_POINT('Ctrl Pts',(0.283214707341173,-0.303141259068211,
1.68332504372461));
#8648=CARTESIAN_POINT('Ctrl Pts',(0.244262842368623,-0.335108247315849,
1.68958170688653));
#8649=CARTESIAN_POINT('Ctrl Pts',(0.178166559972324,-0.373243761060364,
1.69769003172132));
#8650=CARTESIAN_POINT('Ctrl Pts',(0.143648558862931,-0.387888272594439,
1.70107730356824));
#8651=CARTESIAN_POINT('Ctrl Pts',(0.0717778861362652,-0.407041111792943,
1.70562212620408));
#8652=CARTESIAN_POINT('Ctrl Pts',(0.0344244045173309,-0.411552957311693,
1.706752));
#8653=CARTESIAN_POINT('Ctrl Pts',(-0.0344244045173315,-0.411552957311693,
1.706752));
#8654=CARTESIAN_POINT('Ctrl Pts',(-0.0717778861362658,-0.407041111792943,
1.70562212620408));
#8655=CARTESIAN_POINT('Ctrl Pts',(-0.143648558862932,-0.387888272594439,
1.70107730356824));
#8656=CARTESIAN_POINT('Ctrl Pts',(-0.178166559972325,-0.373243761060364,
1.69769003172132));
#8657=CARTESIAN_POINT('Ctrl Pts',(-0.244262842368624,-0.335108247315849,
1.68958170688653));
#8658=CARTESIAN_POINT('Ctrl Pts',(-0.283214707341173,-0.303141259068212,
1.68332504372461));
#8659=CARTESIAN_POINT('Ctrl Pts',(-0.341837165343982,-0.236152929235937,
1.67246562047521));
#8660=CARTESIAN_POINT('Ctrl Pts',(-0.368536561654408,-0.192480977588835,
1.66658649961961));
#8661=CARTESIAN_POINT('Ctrl Pts',(-0.394174530911059,-0.123823518623745,
1.66063136041479));
#8662=CARTESIAN_POINT('Ctrl Pts',(-0.400393769631748,-0.101649918886749,
1.65912839404491));
#8663=CARTESIAN_POINT('Ctrl Pts',(-0.404717578595297,-0.0793800000000001,
1.65807299932179));
#8664=CARTESIAN_POINT('',(-0.886256117232624,-0.07938,1.45861320581289));
#8665=CARTESIAN_POINT('Origin',(0.,-0.07938,0.));
#8666=CARTESIAN_POINT('',(-1.45861320581289,-0.07938,0.886256117232623));
#8667=CARTESIAN_POINT('Ctrl Pts',(-0.886256117232623,-0.0793800000000001,
1.45861320581289));
#8668=CARTESIAN_POINT('Ctrl Pts',(-0.890059788636852,-0.101649918886749,
1.45630208793976));
#8669=CARTESIAN_POINT('Ctrl Pts',(-0.895520212222106,-0.123823518623745,
1.45296717977858));
#8670=CARTESIAN_POINT('Ctrl Pts',(-0.917859913453974,-0.192480977588835,
1.43904931717599));
#8671=CARTESIAN_POINT('Ctrl Pts',(-0.940896403863071,-0.236152929235937,
1.4243271592157));
#8672=CARTESIAN_POINT('Ctrl Pts',(-0.990027513266105,-0.303141259068211,
1.39055359345152));
#8673=CARTESIAN_POINT('Ctrl Pts',(-1.02199477007745,-0.335108247315848,
1.36743459453896));
#8674=CARTESIAN_POINT('Ctrl Pts',(-1.07446535104584,-0.373243761060364,
1.32643091652006));
#8675=CARTESIAN_POINT('Ctrl Pts',(-1.10126842659597,-0.387888272594439,
1.30441816675528));
#8676=CARTESIAN_POINT('Ctrl Pts',(-1.15530234155453,-0.407041111792943,
1.25681160160691));
#8677=CARTESIAN_POINT('Ctrl Pts',(-1.18251418313119,-0.411552957311693,
1.23119764287622));
#8678=CARTESIAN_POINT('Ctrl Pts',(-1.23119764287622,-0.411552957311693,
1.18251418313119));
#8679=CARTESIAN_POINT('Ctrl Pts',(-1.25681160160691,-0.407041111792943,
1.15530234155453));
#8680=CARTESIAN_POINT('Ctrl Pts',(-1.30441816675528,-0.387888272594439,
1.10126842659597));
#8681=CARTESIAN_POINT('Ctrl Pts',(-1.32643091652006,-0.373243761060365,
1.07446535104584));
#8682=CARTESIAN_POINT('Ctrl Pts',(-1.36743459453896,-0.335108247315849,
1.02199477007745));
#8683=CARTESIAN_POINT('Ctrl Pts',(-1.39055359345152,-0.303141259068212,
0.990027513266106));
#8684=CARTESIAN_POINT('Ctrl Pts',(-1.4243271592157,-0.236152929235938,0.940896403863071));
#8685=CARTESIAN_POINT('Ctrl Pts',(-1.43904931717599,-0.192480977588836,
0.917859913453974));
#8686=CARTESIAN_POINT('Ctrl Pts',(-1.45296717977858,-0.123823518623746,
0.895520212222106));
#8687=CARTESIAN_POINT('Ctrl Pts',(-1.45630208793976,-0.101649918886749,
0.890059788636852));
#8688=CARTESIAN_POINT('Ctrl Pts',(-1.45861320581289,-0.0793800000000001,
0.886256117232623));
#8689=CARTESIAN_POINT('',(-1.65807299932179,-0.07938,0.404717578595295));
#8690=CARTESIAN_POINT('Origin',(0.,-0.07938,0.));
#8691=CARTESIAN_POINT('',(-1.706752,-0.411552957311693,2.08591827245526E-16));
#8692=CARTESIAN_POINT('Ctrl Pts',(-1.65807299932179,-0.0793800000000001,
0.404717578595296));
#8693=CARTESIAN_POINT('Ctrl Pts',(-1.65912839404491,-0.101649918886749,
0.400393769631747));
#8694=CARTESIAN_POINT('Ctrl Pts',(-1.66063136041479,-0.123823518623745,
0.394174530911058));
#8695=CARTESIAN_POINT('Ctrl Pts',(-1.66658649961961,-0.192480977588835,
0.368536561654407));
#8696=CARTESIAN_POINT('Ctrl Pts',(-1.67246562047521,-0.236152929235937,
0.341837165343982));
#8697=CARTESIAN_POINT('Ctrl Pts',(-1.68332504372461,-0.303141259068211,
0.283214707341173));
#8698=CARTESIAN_POINT('Ctrl Pts',(-1.68958170688653,-0.335108247315848,
0.244262842368623));
#8699=CARTESIAN_POINT('Ctrl Pts',(-1.69769003172132,-0.373243761060364,
0.178166559972324));
#8700=CARTESIAN_POINT('Ctrl Pts',(-1.70107730356824,-0.387888272594439,
0.143648558862931));
#8701=CARTESIAN_POINT('Ctrl Pts',(-1.70562212620408,-0.407041111792943,
0.0717778861362656));
#8702=CARTESIAN_POINT('Ctrl Pts',(-1.706752,-0.411552957311693,0.0344244045173313));
#8703=CARTESIAN_POINT('Ctrl Pts',(-1.706752,-0.411552957311693,2.08166817117217E-16));
#8704=CARTESIAN_POINT('',(-1.706752,-0.47628,2.09016837373834E-16));
#8705=CARTESIAN_POINT('',(-1.706752,-0.27783,2.09016837373834E-16));
#8706=CARTESIAN_POINT('Origin',(0.,-0.47628,0.));
#8707=CARTESIAN_POINT('',(-1.65807299932179,-0.07938,-0.404717578595296));
#8708=CARTESIAN_POINT('Ctrl Pts',(-1.706752,-0.411552957311693,2.0122792321331E-16));
#8709=CARTESIAN_POINT('Ctrl Pts',(-1.706752,-0.411552957311693,-0.0344244045173309));
#8710=CARTESIAN_POINT('Ctrl Pts',(-1.70562212620408,-0.407041111792943,
-0.0717778861362652));
#8711=CARTESIAN_POINT('Ctrl Pts',(-1.70107730356824,-0.387888272594439,
-0.143648558862931));
#8712=CARTESIAN_POINT('Ctrl Pts',(-1.69769003172132,-0.373243761060365,
-0.178166559972324));
#8713=CARTESIAN_POINT('Ctrl Pts',(-1.68958170688653,-0.335108247315849,
-0.244262842368623));
#8714=CARTESIAN_POINT('Ctrl Pts',(-1.68332504372461,-0.303141259068212,
-0.283214707341173));
#8715=CARTESIAN_POINT('Ctrl Pts',(-1.67246562047521,-0.236152929235938,
-0.341837165343982));
#8716=CARTESIAN_POINT('Ctrl Pts',(-1.66658649961961,-0.192480977588836,
-0.368536561654407));
#8717=CARTESIAN_POINT('Ctrl Pts',(-1.66063136041479,-0.123823518623745,
-0.394174530911059));
#8718=CARTESIAN_POINT('Ctrl Pts',(-1.65912839404491,-0.101649918886749,
-0.400393769631748));
#8719=CARTESIAN_POINT('Ctrl Pts',(-1.65807299932179,-0.0793800000000001,
-0.404717578595296));
#8720=CARTESIAN_POINT('',(-1.45861320581289,-0.07938,-0.886256117232623));
#8721=CARTESIAN_POINT('Origin',(0.,-0.07938,0.));
#8722=CARTESIAN_POINT('',(-0.886256117232623,-0.07938,-1.45861320581289));
#8723=CARTESIAN_POINT('Ctrl Pts',(-1.45861320581289,-0.0793800000000001,
-0.886256117232623));
#8724=CARTESIAN_POINT('Ctrl Pts',(-1.45630208793976,-0.101649918886749,
-0.890059788636852));
#8725=CARTESIAN_POINT('Ctrl Pts',(-1.45296717977858,-0.123823518623745,
-0.895520212222106));
#8726=CARTESIAN_POINT('Ctrl Pts',(-1.43904931717599,-0.192480977588835,
-0.917859913453974));
#8727=CARTESIAN_POINT('Ctrl Pts',(-1.4243271592157,-0.236152929235937,-0.940896403863072));
#8728=CARTESIAN_POINT('Ctrl Pts',(-1.39055359345152,-0.303141259068212,
-0.990027513266106));
#8729=CARTESIAN_POINT('Ctrl Pts',(-1.36743459453896,-0.335108247315849,
-1.02199477007745));
#8730=CARTESIAN_POINT('Ctrl Pts',(-1.32643091652006,-0.373243761060364,
-1.07446535104584));
#8731=CARTESIAN_POINT('Ctrl Pts',(-1.30441816675528,-0.387888272594439,
-1.10126842659597));
#8732=CARTESIAN_POINT('Ctrl Pts',(-1.25681160160691,-0.407041111792943,
-1.15530234155453));
#8733=CARTESIAN_POINT('Ctrl Pts',(-1.23119764287622,-0.411552957311693,
-1.18251418313119));
#8734=CARTESIAN_POINT('Ctrl Pts',(-1.18251418313119,-0.411552957311693,
-1.23119764287622));
#8735=CARTESIAN_POINT('Ctrl Pts',(-1.15530234155453,-0.407041111792943,
-1.25681160160691));
#8736=CARTESIAN_POINT('Ctrl Pts',(-1.10126842659597,-0.387888272594439,
-1.30441816675528));
#8737=CARTESIAN_POINT('Ctrl Pts',(-1.07446535104584,-0.373243761060364,
-1.32643091652006));
#8738=CARTESIAN_POINT('Ctrl Pts',(-1.02199477007745,-0.335108247315848,
-1.36743459453896));
#8739=CARTESIAN_POINT('Ctrl Pts',(-0.990027513266105,-0.303141259068211,
-1.39055359345152));
#8740=CARTESIAN_POINT('Ctrl Pts',(-0.940896403863071,-0.236152929235936,
-1.42432715921571));
#8741=CARTESIAN_POINT('Ctrl Pts',(-0.917859913453974,-0.192480977588835,
-1.43904931717599));
#8742=CARTESIAN_POINT('Ctrl Pts',(-0.895520212222106,-0.123823518623745,
-1.45296717977858));
#8743=CARTESIAN_POINT('Ctrl Pts',(-0.890059788636851,-0.101649918886749,
-1.45630208793976));
#8744=CARTESIAN_POINT('Ctrl Pts',(-0.886256117232623,-0.0793800000000001,
-1.45861320581289));
#8745=CARTESIAN_POINT('',(-0.404717578595295,-0.07938,-1.65807299932179));
#8746=CARTESIAN_POINT('Origin',(0.,-0.07938,0.));
#8747=CARTESIAN_POINT('',(0.404717578595296,-0.07938,-1.65807299932179));
#8748=CARTESIAN_POINT('Ctrl Pts',(-0.404717578595296,-0.0793800000000001,
-1.65807299932179));
#8749=CARTESIAN_POINT('Ctrl Pts',(-0.400393769631747,-0.101649918886749,
-1.65912839404491));
#8750=CARTESIAN_POINT('Ctrl Pts',(-0.394174530911058,-0.123823518623746,
-1.66063136041479));
#8751=CARTESIAN_POINT('Ctrl Pts',(-0.368536561654407,-0.192480977588836,
-1.66658649961961));
#8752=CARTESIAN_POINT('Ctrl Pts',(-0.341837165343982,-0.236152929235938,
-1.67246562047521));
#8753=CARTESIAN_POINT('Ctrl Pts',(-0.283214707341173,-0.303141259068212,
-1.68332504372461));
#8754=CARTESIAN_POINT('Ctrl Pts',(-0.244262842368623,-0.335108247315849,
-1.68958170688653));
#8755=CARTESIAN_POINT('Ctrl Pts',(-0.178166559972324,-0.373243761060364,
-1.69769003172132));
#8756=CARTESIAN_POINT('Ctrl Pts',(-0.143648558862931,-0.387888272594439,
-1.70107730356824));
#8757=CARTESIAN_POINT('Ctrl Pts',(-0.0717778861362653,-0.407041111792943,
-1.70562212620408));
#8758=CARTESIAN_POINT('Ctrl Pts',(-0.034424404517331,-0.411552957311693,
-1.706752));
#8759=CARTESIAN_POINT('Ctrl Pts',(0.0344244045173312,-0.411552957311693,
-1.706752));
#8760=CARTESIAN_POINT('Ctrl Pts',(0.0717778861362655,-0.407041111792943,
-1.70562212620408));
#8761=CARTESIAN_POINT('Ctrl Pts',(0.143648558862931,-0.387888272594439,
-1.70107730356824));
#8762=CARTESIAN_POINT('Ctrl Pts',(0.178166559972324,-0.373243761060364,
-1.69769003172132));
#8763=CARTESIAN_POINT('Ctrl Pts',(0.244262842368623,-0.335108247315849,
-1.68958170688653));
#8764=CARTESIAN_POINT('Ctrl Pts',(0.283214707341173,-0.303141259068212,
-1.68332504372461));
#8765=CARTESIAN_POINT('Ctrl Pts',(0.341837165343982,-0.236152929235937,
-1.67246562047521));
#8766=CARTESIAN_POINT('Ctrl Pts',(0.368536561654407,-0.192480977588835,
-1.66658649961961));
#8767=CARTESIAN_POINT('Ctrl Pts',(0.394174530911059,-0.123823518623745,
-1.66063136041479));
#8768=CARTESIAN_POINT('Ctrl Pts',(0.400393769631748,-0.101649918886749,
-1.65912839404491));
#8769=CARTESIAN_POINT('Ctrl Pts',(0.404717578595296,-0.0793800000000001,
-1.65807299932179));
#8770=CARTESIAN_POINT('',(0.886256117232623,-0.07938,-1.45861320581289));
#8771=CARTESIAN_POINT('Origin',(0.,-0.07938,0.));
#8772=CARTESIAN_POINT('',(1.45861320581289,-0.07938,-0.886256117232623));
#8773=CARTESIAN_POINT('Ctrl Pts',(0.886256117232623,-0.0793800000000001,
-1.45861320581289));
#8774=CARTESIAN_POINT('Ctrl Pts',(0.890059788636852,-0.101649918886749,
-1.45630208793976));
#8775=CARTESIAN_POINT('Ctrl Pts',(0.895520212222106,-0.123823518623745,
-1.45296717977858));
#8776=CARTESIAN_POINT('Ctrl Pts',(0.917859913453974,-0.192480977588835,
-1.43904931717599));
#8777=CARTESIAN_POINT('Ctrl Pts',(0.940896403863072,-0.236152929235937,
-1.4243271592157));
#8778=CARTESIAN_POINT('Ctrl Pts',(0.990027513266106,-0.303141259068211,
-1.39055359345152));
#8779=CARTESIAN_POINT('Ctrl Pts',(1.02199477007745,-0.335108247315849,-1.36743459453896));
#8780=CARTESIAN_POINT('Ctrl Pts',(1.07446535104584,-0.373243761060364,-1.32643091652006));
#8781=CARTESIAN_POINT('Ctrl Pts',(1.10126842659597,-0.387888272594439,-1.30441816675528));
#8782=CARTESIAN_POINT('Ctrl Pts',(1.15530234155453,-0.407041111792943,-1.25681160160691));
#8783=CARTESIAN_POINT('Ctrl Pts',(1.18251418313119,-0.411552957311693,-1.23119764287622));
#8784=CARTESIAN_POINT('Ctrl Pts',(1.23119764287622,-0.411552957311693,-1.18251418313119));
#8785=CARTESIAN_POINT('Ctrl Pts',(1.25681160160691,-0.407041111792943,-1.15530234155453));
#8786=CARTESIAN_POINT('Ctrl Pts',(1.30441816675528,-0.387888272594439,-1.10126842659597));
#8787=CARTESIAN_POINT('Ctrl Pts',(1.32643091652006,-0.373243761060364,-1.07446535104584));
#8788=CARTESIAN_POINT('Ctrl Pts',(1.36743459453896,-0.335108247315849,-1.02199477007745));
#8789=CARTESIAN_POINT('Ctrl Pts',(1.39055359345152,-0.303141259068212,-0.990027513266105));
#8790=CARTESIAN_POINT('Ctrl Pts',(1.4243271592157,-0.236152929235937,-0.940896403863071));
#8791=CARTESIAN_POINT('Ctrl Pts',(1.43904931717599,-0.192480977588835,-0.917859913453974));
#8792=CARTESIAN_POINT('Ctrl Pts',(1.45296717977858,-0.123823518623745,-0.895520212222106));
#8793=CARTESIAN_POINT('Ctrl Pts',(1.45630208793976,-0.101649918886749,-0.890059788636852));
#8794=CARTESIAN_POINT('Ctrl Pts',(1.45861320581289,-0.0793800000000001,
-0.886256117232623));
#8795=CARTESIAN_POINT('',(1.65807299932179,-0.07938,-0.404717578595296));
#8796=CARTESIAN_POINT('Origin',(0.,-0.07938,0.));
#8797=CARTESIAN_POINT('',(1.65807299932179,-0.07938,0.404717578595296));
#8798=CARTESIAN_POINT('Ctrl Pts',(1.65807299932179,-0.0793800000000001,
-0.404717578595296));
#8799=CARTESIAN_POINT('Ctrl Pts',(1.65912839404491,-0.101649918886749,-0.400393769631747));
#8800=CARTESIAN_POINT('Ctrl Pts',(1.66063136041479,-0.123823518623745,-0.394174530911058));
#8801=CARTESIAN_POINT('Ctrl Pts',(1.66658649961961,-0.192480977588835,-0.368536561654407));
#8802=CARTESIAN_POINT('Ctrl Pts',(1.67246562047521,-0.236152929235937,-0.341837165343982));
#8803=CARTESIAN_POINT('Ctrl Pts',(1.68332504372461,-0.303141259068212,-0.283214707341173));
#8804=CARTESIAN_POINT('Ctrl Pts',(1.68958170688653,-0.335108247315849,-0.244262842368623));
#8805=CARTESIAN_POINT('Ctrl Pts',(1.69769003172132,-0.373243761060364,-0.178166559972324));
#8806=CARTESIAN_POINT('Ctrl Pts',(1.70107730356824,-0.387888272594439,-0.143648558862931));
#8807=CARTESIAN_POINT('Ctrl Pts',(1.70562212620408,-0.407041111792943,-0.0717778861362655));
#8808=CARTESIAN_POINT('Ctrl Pts',(1.706752,-0.411552957311693,-0.0344244045173312));
#8809=CARTESIAN_POINT('Ctrl Pts',(1.706752,-0.411552957311693,0.0344244045173312));
#8810=CARTESIAN_POINT('Ctrl Pts',(1.70562212620408,-0.407041111792943,0.0717778861362655));
#8811=CARTESIAN_POINT('Ctrl Pts',(1.70107730356824,-0.387888272594439,0.143648558862931));
#8812=CARTESIAN_POINT('Ctrl Pts',(1.69769003172132,-0.373243761060364,0.178166559972324));
#8813=CARTESIAN_POINT('Ctrl Pts',(1.68958170688653,-0.335108247315849,0.244262842368623));
#8814=CARTESIAN_POINT('Ctrl Pts',(1.68332504372461,-0.303141259068212,0.283214707341173));
#8815=CARTESIAN_POINT('Ctrl Pts',(1.67246562047521,-0.236152929235937,0.341837165343982));
#8816=CARTESIAN_POINT('Ctrl Pts',(1.66658649961961,-0.192480977588835,0.368536561654407));
#8817=CARTESIAN_POINT('Ctrl Pts',(1.66063136041479,-0.123823518623745,0.394174530911058));
#8818=CARTESIAN_POINT('Ctrl Pts',(1.65912839404491,-0.101649918886749,0.400393769631747));
#8819=CARTESIAN_POINT('Ctrl Pts',(1.65807299932179,-0.0793800000000001,
0.404717578595296));
#8820=CARTESIAN_POINT('Origin',(0.,-0.07938,0.));
#8821=CARTESIAN_POINT('Origin',(0.,-0.07938,0.));
#8822=CARTESIAN_POINT('',(0.397005914195118,-0.07938,1.59456899932179));
#8823=CARTESIAN_POINT('Origin',(0.,-0.07938,0.));
#8824=CARTESIAN_POINT('Origin',(-3.33066907387547E-16,-0.07938,1.675));
#8825=CARTESIAN_POINT('Origin',(-3.33066907387547E-16,0.,1.675));
#8826=CARTESIAN_POINT('',(-0.397005914195118,-0.07938,1.59456899932179));
#8827=CARTESIAN_POINT('Ctrl Pts',(-0.397005914195119,-0.0793800000000001,
1.59456899932179));
#8828=CARTESIAN_POINT('Ctrl Pts',(-0.3886265584581,-0.123401821157026,1.59665523941937));
#8829=CARTESIAN_POINT('Ctrl Pts',(-0.373030350867485,-0.166543350814306,
1.60050712143809));
#8830=CARTESIAN_POINT('Ctrl Pts',(-0.333298652394954,-0.237231147975234,
1.60919314384089));
#8831=CARTESIAN_POINT('Ctrl Pts',(-0.311480544243687,-0.266264900654909,
1.61365775139403));
#8832=CARTESIAN_POINT('Ctrl Pts',(-0.261368388670537,-0.317195968905306,
1.62252828437015));
#8833=CARTESIAN_POINT('Ctrl Pts',(-0.233069203882014,-0.33909093068465,
1.62691869420078));
#8834=CARTESIAN_POINT('Ctrl Pts',(-0.174042761838764,-0.373586846396559,
1.63426473152765));
#8835=CARTESIAN_POINT('Ctrl Pts',(-0.14036578147155,-0.388086240756494,
1.63761964365402));
#8836=CARTESIAN_POINT('Ctrl Pts',(-0.0701778381840615,-0.407068917407805,
1.64212536811722));
#8837=CARTESIAN_POINT('Ctrl Pts',(-0.0336652739555918,-0.411552957311693,
1.643248));
#8838=CARTESIAN_POINT('Ctrl Pts',(0.0336652739555913,-0.411552957311693,
1.643248));
#8839=CARTESIAN_POINT('Ctrl Pts',(0.070177838184061,-0.407068917407805,
1.64212536811722));
#8840=CARTESIAN_POINT('Ctrl Pts',(0.140365781471549,-0.388086240756494,
1.63761964365402));
#8841=CARTESIAN_POINT('Ctrl Pts',(0.174042761838763,-0.373586846396559,
1.63426473152765));
#8842=CARTESIAN_POINT('Ctrl Pts',(0.233069203882014,-0.33909093068465,1.62691869420078));
#8843=CARTESIAN_POINT('Ctrl Pts',(0.261368388670536,-0.317195968905306,
1.62252828437015));
#8844=CARTESIAN_POINT('Ctrl Pts',(0.311480544243686,-0.266264900654908,
1.61365775139403));
#8845=CARTESIAN_POINT('Ctrl Pts',(0.333298652394954,-0.237231147975234,
1.60919314384089));
#8846=CARTESIAN_POINT('Ctrl Pts',(0.373030350867484,-0.166543350814306,
1.60050712143809));
#8847=CARTESIAN_POINT('Ctrl Pts',(0.388626558458099,-0.123401821157026,
1.59665523941937));
#8848=CARTESIAN_POINT('Ctrl Pts',(0.397005914195118,-0.07938,1.59456899932179));
#8849=CARTESIAN_POINT('Origin',(-3.33066907387547E-16,-0.07938,1.675));
#8850=CARTESIAN_POINT('Origin',(0.,-0.07938,0.));
#8851=CARTESIAN_POINT('',(-0.846804978391754,-0.07938,1.40825612658882));
#8852=CARTESIAN_POINT('Origin',(0.,-0.07938,0.));
#8853=CARTESIAN_POINT('Origin',(-1.18440385848747,-0.07938,1.18440385848747));
#8854=CARTESIAN_POINT('Origin',(-1.18440385848747,0.,1.18440385848747));
#8855=CARTESIAN_POINT('',(-1.40825612658882,-0.07938,0.846804978391753));
#8856=CARTESIAN_POINT('Ctrl Pts',(-1.40825612658882,-0.0793800000000001,
0.846804978391753));
#8857=CARTESIAN_POINT('Ctrl Pts',(-1.40380622184538,-0.123401821157026,
0.854205272175555));
#8858=CARTESIAN_POINT('Ctrl Pts',(-1.39550172959303,-0.166543350814306,
0.867957148219442));
#8859=CARTESIAN_POINT('Ctrl Pts',(-1.3735491215176,-0.237231147975235,0.902193646979983));
#8860=CARTESIAN_POINT('Ctrl Pts',(-1.36127834356734,-0.266264900654909,
0.920778333482565));
#8861=CARTESIAN_POINT('Ctrl Pts',(-1.33211611256184,-0.317195968905306,
0.962485392528369));
#8862=CARTESIAN_POINT('Ctrl Pts',(-1.31521005565926,-0.339090930684651,
0.985600426557816));
#8863=CARTESIAN_POINT('Ctrl Pts',(-1.27866649102984,-0.373586846396559,
1.03253285680459));
#8864=CARTESIAN_POINT('Ctrl Pts',(-1.25722555095714,-0.388086240756494,
1.05871835910697));
#8865=CARTESIAN_POINT('Ctrl Pts',(-1.2107812086231,-0.407068917407805,1.11153475808518));
#8866=CARTESIAN_POINT('Ctrl Pts',(-1.18575674747573,-0.411552957311693,
1.13814686046673));
#8867=CARTESIAN_POINT('Ctrl Pts',(-1.13814686046673,-0.411552957311693,
1.18575674747573));
#8868=CARTESIAN_POINT('Ctrl Pts',(-1.11153475808518,-0.407068917407805,
1.2107812086231));
#8869=CARTESIAN_POINT('Ctrl Pts',(-1.05871835910697,-0.388086240756494,
1.25722555095714));
#8870=CARTESIAN_POINT('Ctrl Pts',(-1.03253285680459,-0.373586846396559,
1.27866649102984));
#8871=CARTESIAN_POINT('Ctrl Pts',(-0.985600426557816,-0.33909093068465,
1.31521005565926));
#8872=CARTESIAN_POINT('Ctrl Pts',(-0.962485392528369,-0.317195968905306,
1.33211611256184));
#8873=CARTESIAN_POINT('Ctrl Pts',(-0.920778333482565,-0.266264900654908,
1.36127834356734));
#8874=CARTESIAN_POINT('Ctrl Pts',(-0.902193646979983,-0.237231147975234,
1.3735491215176));
#8875=CARTESIAN_POINT('Ctrl Pts',(-0.867957148219442,-0.166543350814306,
1.39550172959303));
#8876=CARTESIAN_POINT('Ctrl Pts',(-0.854205272175555,-0.123401821157026,
1.40380622184538));
#8877=CARTESIAN_POINT('Ctrl Pts',(-0.846804978391753,-0.0793800000000001,
1.40825612658882));
#8878=CARTESIAN_POINT('Origin',(-1.18440385848747,-0.07938,1.18440385848747));
#8879=CARTESIAN_POINT('Origin',(0.,-0.07938,0.));
#8880=CARTESIAN_POINT('',(-1.59456899932179,-0.07938,0.397005914195118));
#8881=CARTESIAN_POINT('Origin',(0.,-0.07938,0.));
#8882=CARTESIAN_POINT('Origin',(-1.675,-0.07938,-2.22044604925031E-16));
#8883=CARTESIAN_POINT('Origin',(-1.675,0.,-2.22044604925031E-16));
#8884=CARTESIAN_POINT('',(-1.59456899932179,-0.07938,-0.397005914195118));
#8885=CARTESIAN_POINT('',(-1.643248,-0.411552957311693,3.47540551556327E-18));
#8886=CARTESIAN_POINT('Ctrl Pts',(-1.59456899932179,-0.0793800000000001,
-0.397005914195119));
#8887=CARTESIAN_POINT('Ctrl Pts',(-1.59665523941937,-0.123401821157026,
-0.388626558458099));
#8888=CARTESIAN_POINT('Ctrl Pts',(-1.60050712143809,-0.166543350814306,
-0.373030350867485));
#8889=CARTESIAN_POINT('Ctrl Pts',(-1.60919314384089,-0.237231147975234,
-0.333298652394954));
#8890=CARTESIAN_POINT('Ctrl Pts',(-1.61365775139403,-0.266264900654909,
-0.311480544243686));
#8891=CARTESIAN_POINT('Ctrl Pts',(-1.62252828437015,-0.317195968905306,
-0.261368388670537));
#8892=CARTESIAN_POINT('Ctrl Pts',(-1.62691869420078,-0.33909093068465,-0.233069203882014));
#8893=CARTESIAN_POINT('Ctrl Pts',(-1.63426473152765,-0.373586846396559,
-0.174042761838764));
#8894=CARTESIAN_POINT('Ctrl Pts',(-1.63761964365402,-0.388086240756494,
-0.140365781471549));
#8895=CARTESIAN_POINT('Ctrl Pts',(-1.64212536811722,-0.407068917407805,
-0.0701778381840614));
#8896=CARTESIAN_POINT('Ctrl Pts',(-1.643248,-0.411552957311693,-0.0336652739555917));
#8897=CARTESIAN_POINT('Ctrl Pts',(-1.643248,-0.411552957311693,-2.0122792321331E-16));
#8898=CARTESIAN_POINT('Origin',(-1.675,-0.07938,-2.22044604925031E-16));
#8899=CARTESIAN_POINT('Ctrl Pts',(-1.643248,-0.411552957311693,-1.94289029309402E-16));
#8900=CARTESIAN_POINT('Ctrl Pts',(-1.643248,-0.411552957311693,0.0336652739555913));
#8901=CARTESIAN_POINT('Ctrl Pts',(-1.64212536811722,-0.407068917407805,
0.0701778381840609));
#8902=CARTESIAN_POINT('Ctrl Pts',(-1.63761964365402,-0.388086240756494,
0.140365781471549));
#8903=CARTESIAN_POINT('Ctrl Pts',(-1.63426473152765,-0.373586846396559,
0.174042761838763));
#8904=CARTESIAN_POINT('Ctrl Pts',(-1.62691869420078,-0.33909093068465,0.233069203882014));
#8905=CARTESIAN_POINT('Ctrl Pts',(-1.62252828437015,-0.317195968905306,
0.261368388670536));
#8906=CARTESIAN_POINT('Ctrl Pts',(-1.61365775139403,-0.266264900654909,
0.311480544243686));
#8907=CARTESIAN_POINT('Ctrl Pts',(-1.60919314384089,-0.237231147975235,
0.333298652394954));
#8908=CARTESIAN_POINT('Ctrl Pts',(-1.60050712143809,-0.166543350814306,
0.373030350867484));
#8909=CARTESIAN_POINT('Ctrl Pts',(-1.59665523941937,-0.123401821157026,
0.388626558458099));
#8910=CARTESIAN_POINT('Ctrl Pts',(-1.59456899932179,-0.0793800000000001,
0.397005914195118));
#8911=CARTESIAN_POINT('Origin',(0.,-0.07938,0.));
#8912=CARTESIAN_POINT('',(-1.40825612658882,-0.07938,-0.846804978391753));
#8913=CARTESIAN_POINT('Origin',(0.,-0.07938,0.));
#8914=CARTESIAN_POINT('Origin',(-1.18440385848747,-0.07938,-1.18440385848747));
#8915=CARTESIAN_POINT('Origin',(-1.18440385848747,0.,-1.18440385848747));
#8916=CARTESIAN_POINT('',(-0.846804978391753,-0.07938,-1.40825612658882));
#8917=CARTESIAN_POINT('Ctrl Pts',(-0.846804978391753,-0.0793800000000001,
-1.40825612658882));
#8918=CARTESIAN_POINT('Ctrl Pts',(-0.854205272175555,-0.123401821157026,
-1.40380622184538));
#8919=CARTESIAN_POINT('Ctrl Pts',(-0.867957148219442,-0.166543350814306,
-1.39550172959303));
#8920=CARTESIAN_POINT('Ctrl Pts',(-0.902193646979982,-0.237231147975234,
-1.3735491215176));
#8921=CARTESIAN_POINT('Ctrl Pts',(-0.920778333482564,-0.266264900654908,
-1.36127834356734));
#8922=CARTESIAN_POINT('Ctrl Pts',(-0.962485392528368,-0.317195968905306,
-1.33211611256184));
#8923=CARTESIAN_POINT('Ctrl Pts',(-0.985600426557816,-0.33909093068465,
-1.31521005565926));
#8924=CARTESIAN_POINT('Ctrl Pts',(-1.03253285680459,-0.373586846396559,
-1.27866649102984));
#8925=CARTESIAN_POINT('Ctrl Pts',(-1.05871835910697,-0.388086240756494,
-1.25722555095714));
#8926=CARTESIAN_POINT('Ctrl Pts',(-1.11153475808518,-0.407068917407805,
-1.2107812086231));
#8927=CARTESIAN_POINT('Ctrl Pts',(-1.13814686046673,-0.411552957311693,
-1.18575674747573));
#8928=CARTESIAN_POINT('Ctrl Pts',(-1.18575674747573,-0.411552957311693,
-1.13814686046673));
#8929=CARTESIAN_POINT('Ctrl Pts',(-1.2107812086231,-0.407068917407805,-1.11153475808518));
#8930=CARTESIAN_POINT('Ctrl Pts',(-1.25722555095714,-0.388086240756494,
-1.05871835910697));
#8931=CARTESIAN_POINT('Ctrl Pts',(-1.27866649102984,-0.373586846396559,
-1.03253285680459));
#8932=CARTESIAN_POINT('Ctrl Pts',(-1.31521005565926,-0.33909093068465,-0.985600426557816));
#8933=CARTESIAN_POINT('Ctrl Pts',(-1.33211611256184,-0.317195968905306,
-0.962485392528369));
#8934=CARTESIAN_POINT('Ctrl Pts',(-1.36127834356734,-0.266264900654909,
-0.920778333482565));
#8935=CARTESIAN_POINT('Ctrl Pts',(-1.3735491215176,-0.237231147975234,-0.902193646979983));
#8936=CARTESIAN_POINT('Ctrl Pts',(-1.39550172959303,-0.166543350814306,
-0.867957148219442));
#8937=CARTESIAN_POINT('Ctrl Pts',(-1.40380622184538,-0.123401821157026,
-0.854205272175555));
#8938=CARTESIAN_POINT('Ctrl Pts',(-1.40825612658882,-0.07938,-0.846804978391753));
#8939=CARTESIAN_POINT('Origin',(-1.18440385848747,-0.07938,-1.18440385848747));
#8940=CARTESIAN_POINT('Origin',(0.,-0.07938,0.));
#8941=CARTESIAN_POINT('',(-0.397005914195118,-0.07938,-1.59456899932179));
#8942=CARTESIAN_POINT('Origin',(0.,-0.07938,0.));
#8943=CARTESIAN_POINT('Origin',(1.11022302462516E-16,-0.07938,-1.675));
#8944=CARTESIAN_POINT('Origin',(1.11022302462516E-16,0.,-1.675));
#8945=CARTESIAN_POINT('',(0.397005914195118,-0.07938,-1.59456899932179));
#8946=CARTESIAN_POINT('Ctrl Pts',(0.397005914195119,-0.0793800000000001,
-1.59456899932179));
#8947=CARTESIAN_POINT('Ctrl Pts',(0.388626558458099,-0.123401821157026,
-1.59665523941937));
#8948=CARTESIAN_POINT('Ctrl Pts',(0.373030350867485,-0.166543350814306,
-1.60050712143809));
#8949=CARTESIAN_POINT('Ctrl Pts',(0.333298652394954,-0.237231147975234,
-1.60919314384089));
#8950=CARTESIAN_POINT('Ctrl Pts',(0.311480544243686,-0.266264900654909,
-1.61365775139403));
#8951=CARTESIAN_POINT('Ctrl Pts',(0.261368388670537,-0.317195968905306,
-1.62252828437015));
#8952=CARTESIAN_POINT('Ctrl Pts',(0.233069203882014,-0.33909093068465,-1.62691869420078));
#8953=CARTESIAN_POINT('Ctrl Pts',(0.174042761838763,-0.373586846396559,
-1.63426473152765));
#8954=CARTESIAN_POINT('Ctrl Pts',(0.140365781471549,-0.388086240756494,
-1.63761964365402));
#8955=CARTESIAN_POINT('Ctrl Pts',(0.0701778381840612,-0.407068917407805,
-1.64212536811722));
#8956=CARTESIAN_POINT('Ctrl Pts',(0.0336652739555916,-0.411552957311693,
-1.643248));
#8957=CARTESIAN_POINT('Ctrl Pts',(-0.0336652739555915,-0.411552957311693,
-1.643248));
#8958=CARTESIAN_POINT('Ctrl Pts',(-0.0701778381840612,-0.407068917407805,
-1.64212536811722));
#8959=CARTESIAN_POINT('Ctrl Pts',(-0.140365781471549,-0.388086240756494,
-1.63761964365402));
#8960=CARTESIAN_POINT('Ctrl Pts',(-0.174042761838764,-0.373586846396559,
-1.63426473152765));
#8961=CARTESIAN_POINT('Ctrl Pts',(-0.233069203882014,-0.33909093068465,
-1.62691869420078));
#8962=CARTESIAN_POINT('Ctrl Pts',(-0.261368388670536,-0.317195968905306,
-1.62252828437015));
#8963=CARTESIAN_POINT('Ctrl Pts',(-0.311480544243686,-0.266264900654908,
-1.61365775139403));
#8964=CARTESIAN_POINT('Ctrl Pts',(-0.333298652394954,-0.237231147975234,
-1.60919314384089));
#8965=CARTESIAN_POINT('Ctrl Pts',(-0.373030350867485,-0.166543350814306,
-1.60050712143809));
#8966=CARTESIAN_POINT('Ctrl Pts',(-0.388626558458099,-0.123401821157026,
-1.59665523941937));
#8967=CARTESIAN_POINT('Ctrl Pts',(-0.397005914195118,-0.07938,-1.59456899932179));
#8968=CARTESIAN_POINT('Origin',(1.11022302462516E-16,-0.07938,-1.675));
#8969=CARTESIAN_POINT('Origin',(0.,-0.07938,0.));
#8970=CARTESIAN_POINT('',(0.846804978391753,-0.07938,-1.40825612658882));
#8971=CARTESIAN_POINT('Origin',(0.,-0.07938,0.));
#8972=CARTESIAN_POINT('Origin',(1.18440385848747,-0.07938,-1.18440385848747));
#8973=CARTESIAN_POINT('Origin',(1.18440385848747,0.,-1.18440385848747));
#8974=CARTESIAN_POINT('',(1.40825612658882,-0.07938,-0.846804978391753));
#8975=CARTESIAN_POINT('Ctrl Pts',(1.40825612658882,-0.0793800000000001,
-0.846804978391753));
#8976=CARTESIAN_POINT('Ctrl Pts',(1.40380622184538,-0.123401821157026,-0.854205272175555));
#8977=CARTESIAN_POINT('Ctrl Pts',(1.39550172959303,-0.166543350814306,-0.867957148219442));
#8978=CARTESIAN_POINT('Ctrl Pts',(1.3735491215176,-0.237231147975234,-0.902193646979983));
#8979=CARTESIAN_POINT('Ctrl Pts',(1.36127834356734,-0.266264900654908,-0.920778333482565));
#8980=CARTESIAN_POINT('Ctrl Pts',(1.33211611256184,-0.317195968905306,-0.962485392528369));
#8981=CARTESIAN_POINT('Ctrl Pts',(1.31521005565926,-0.33909093068465,-0.985600426557816));
#8982=CARTESIAN_POINT('Ctrl Pts',(1.27866649102984,-0.373586846396559,-1.03253285680459));
#8983=CARTESIAN_POINT('Ctrl Pts',(1.25722555095714,-0.388086240756494,-1.05871835910697));
#8984=CARTESIAN_POINT('Ctrl Pts',(1.2107812086231,-0.407068917407805,-1.11153475808518));
#8985=CARTESIAN_POINT('Ctrl Pts',(1.18575674747573,-0.411552957311693,-1.13814686046673));
#8986=CARTESIAN_POINT('Ctrl Pts',(1.13814686046673,-0.411552957311693,-1.18575674747573));
#8987=CARTESIAN_POINT('Ctrl Pts',(1.11153475808518,-0.407068917407805,-1.2107812086231));
#8988=CARTESIAN_POINT('Ctrl Pts',(1.05871835910697,-0.388086240756494,-1.25722555095714));
#8989=CARTESIAN_POINT('Ctrl Pts',(1.03253285680459,-0.373586846396559,-1.27866649102984));
#8990=CARTESIAN_POINT('Ctrl Pts',(0.985600426557816,-0.33909093068465,-1.31521005565926));
#8991=CARTESIAN_POINT('Ctrl Pts',(0.962485392528369,-0.317195968905306,
-1.33211611256184));
#8992=CARTESIAN_POINT('Ctrl Pts',(0.920778333482565,-0.266264900654909,
-1.36127834356734));
#8993=CARTESIAN_POINT('Ctrl Pts',(0.902193646979983,-0.237231147975234,
-1.3735491215176));
#8994=CARTESIAN_POINT('Ctrl Pts',(0.867957148219442,-0.166543350814306,
-1.39550172959303));
#8995=CARTESIAN_POINT('Ctrl Pts',(0.854205272175555,-0.123401821157026,
-1.40380622184538));
#8996=CARTESIAN_POINT('Ctrl Pts',(0.846804978391753,-0.0793800000000001,
-1.40825612658882));
#8997=CARTESIAN_POINT('Origin',(1.18440385848747,-0.07938,-1.18440385848747));
#8998=CARTESIAN_POINT('Origin',(0.,-0.27783,0.));
#8999=CARTESIAN_POINT('',(-1.643248,-0.47628,2.01239840340529E-16));
#9000=CARTESIAN_POINT('Origin',(0.,-0.47628,0.));
#9001=CARTESIAN_POINT('',(-1.643248,-0.27783,2.01239840340529E-16));
#9002=CARTESIAN_POINT('',(1.59456899932179,-0.07938,0.397005914195118));
#9003=CARTESIAN_POINT('Origin',(0.,-0.07938,0.));
#9004=CARTESIAN_POINT('',(1.59456899932179,-0.07938,-0.397005914195118));
#9005=CARTESIAN_POINT('Ctrl Pts',(1.59456899932179,-0.0793800000000001,
0.397005914195118));
#9006=CARTESIAN_POINT('Ctrl Pts',(1.59665523941937,-0.123401821157026,0.388626558458099));
#9007=CARTESIAN_POINT('Ctrl Pts',(1.60050712143809,-0.166543350814306,0.373030350867485));
#9008=CARTESIAN_POINT('Ctrl Pts',(1.60919314384089,-0.237231147975234,0.333298652394954));
#9009=CARTESIAN_POINT('Ctrl Pts',(1.61365775139403,-0.266264900654909,0.311480544243686));
#9010=CARTESIAN_POINT('Ctrl Pts',(1.62252828437015,-0.317195968905306,0.261368388670537));
#9011=CARTESIAN_POINT('Ctrl Pts',(1.62691869420078,-0.33909093068465,0.233069203882014));
#9012=CARTESIAN_POINT('Ctrl Pts',(1.63426473152765,-0.373586846396559,0.174042761838764));
#9013=CARTESIAN_POINT('Ctrl Pts',(1.63761964365402,-0.388086240756494,0.140365781471549));
#9014=CARTESIAN_POINT('Ctrl Pts',(1.64212536811722,-0.407068917407805,0.0701778381840612));
#9015=CARTESIAN_POINT('Ctrl Pts',(1.643248,-0.411552957311693,0.0336652739555916));
#9016=CARTESIAN_POINT('Ctrl Pts',(1.643248,-0.411552957311693,-0.0336652739555916));
#9017=CARTESIAN_POINT('Ctrl Pts',(1.64212536811722,-0.407068917407805,-0.0701778381840612));
#9018=CARTESIAN_POINT('Ctrl Pts',(1.63761964365402,-0.388086240756494,-0.140365781471549));
#9019=CARTESIAN_POINT('Ctrl Pts',(1.63426473152765,-0.373586846396559,-0.174042761838764));
#9020=CARTESIAN_POINT('Ctrl Pts',(1.62691869420078,-0.33909093068465,-0.233069203882014));
#9021=CARTESIAN_POINT('Ctrl Pts',(1.62252828437015,-0.317195968905306,-0.261368388670537));
#9022=CARTESIAN_POINT('Ctrl Pts',(1.61365775139403,-0.266264900654909,-0.311480544243686));
#9023=CARTESIAN_POINT('Ctrl Pts',(1.60919314384089,-0.237231147975234,-0.333298652394954));
#9024=CARTESIAN_POINT('Ctrl Pts',(1.60050712143809,-0.166543350814306,-0.373030350867485));
#9025=CARTESIAN_POINT('Ctrl Pts',(1.59665523941937,-0.123401821157026,-0.388626558458099));
#9026=CARTESIAN_POINT('Ctrl Pts',(1.59456899932179,-0.07938,-0.397005914195118));
#9027=CARTESIAN_POINT('Origin',(0.,-0.07938,0.));
#9028=CARTESIAN_POINT('Origin',(0.,-0.07938,0.));
#9029=CARTESIAN_POINT('Origin',(1.675,-0.07938,0.));
#9030=CARTESIAN_POINT('Origin',(1.675,0.,0.));
#9031=CARTESIAN_POINT('Origin',(1.675,-0.07938,0.));
#9032=CARTESIAN_POINT('Origin',(0.,-0.47628,0.));
#9033=CARTESIAN_POINT('Origin',(0.,-0.07938,0.));
#9034=CARTESIAN_POINT('',(0.,0.,0.));
#9035=CARTESIAN_POINT('Origin',(1.70469,0.695,0.));
#9036=CARTESIAN_POINT('',(-1.70469,0.695,-2.0876431520385E-16));
#9037=CARTESIAN_POINT('Origin',(0.,0.695,0.));
#9038=CARTESIAN_POINT('',(-1.65031,0.695,-2.02104685910087E-16));
#9039=CARTESIAN_POINT('Origin',(0.,0.695,0.));
#9040=CARTESIAN_POINT('Origin',(0.,0.6575,0.));
#9041=CARTESIAN_POINT('',(-1.70469,0.62,-2.0876431520385E-16));
#9042=CARTESIAN_POINT('Origin',(0.,0.62,0.));
#9043=CARTESIAN_POINT('',(-1.70469,0.6575,-2.0876431520385E-16));
#9044=CARTESIAN_POINT('Origin',(1.65031,0.62,0.));
#9045=CARTESIAN_POINT('',(-1.65031,0.62,-2.02104685910087E-16));
#9046=CARTESIAN_POINT('Origin',(0.,0.62,0.));
#9047=CARTESIAN_POINT('Origin',(0.,0.6575,0.));
#9048=CARTESIAN_POINT('',(-1.65031,0.6575,-2.02104685910087E-16));
#9049=CARTESIAN_POINT('Origin',(1.70469,-0.62,0.));
#9050=CARTESIAN_POINT('',(-1.70469,-0.62,-2.0876431520385E-16));
#9051=CARTESIAN_POINT('Origin',(0.,-0.62,0.));
#9052=CARTESIAN_POINT('',(-1.65031,-0.62,-2.02104685910087E-16));
#9053=CARTESIAN_POINT('Origin',(0.,-0.62,0.));
#9054=CARTESIAN_POINT('Origin',(0.,-0.6575,0.));
#9055=CARTESIAN_POINT('',(-1.70469,-0.695,-2.0876431520385E-16));
#9056=CARTESIAN_POINT('Origin',(0.,-0.695,0.));
#9057=CARTESIAN_POINT('',(-1.70469,-0.6575,-2.0876431520385E-16));
#9058=CARTESIAN_POINT('Origin',(1.65031,-0.695,0.));
#9059=CARTESIAN_POINT('',(-1.65031,-0.695,-2.02104685910087E-16));
#9060=CARTESIAN_POINT('Origin',(0.,-0.695,0.));
#9061=CARTESIAN_POINT('Origin',(0.,-0.6575,0.));
#9062=CARTESIAN_POINT('',(-1.65031,-0.6575,-2.02104685910087E-16));
#9063=CARTESIAN_POINT('',(0.,0.,0.));
#9064=CARTESIAN_POINT('',(0.,0.,0.));
#9065=CARTESIAN_POINT('',(0.,0.,0.));
#9066=CARTESIAN_POINT('',(0.,0.,0.));
#9067=CARTESIAN_POINT('',(0.,0.,0.));
#9068=CARTESIAN_POINT('',(0.,0.,0.));
#9069=CARTESIAN_POINT('Origin',(0.0866025403784439,-0.4,-0.15));
#9070=CARTESIAN_POINT('',(0.173205080756888,-0.4,0.));
#9071=CARTESIAN_POINT('',(0.0866025403784439,-0.4,-0.15));
#9072=CARTESIAN_POINT('',(0.173205080756888,-0.4,0.));
#9073=CARTESIAN_POINT('',(0.0866025403784439,-0.64,-0.15));
#9074=CARTESIAN_POINT('',(0.0866025403784439,-0.4,-0.15));
#9075=CARTESIAN_POINT('',(0.173205080756888,-0.64,0.));
#9076=CARTESIAN_POINT('',(0.173205080756888,-0.64,0.));
#9077=CARTESIAN_POINT('',(0.173205080756888,-0.4,0.));
#9078=CARTESIAN_POINT('Origin',(-0.0866025403784438,-0.4,-0.15));
#9079=CARTESIAN_POINT('',(-0.0866025403784438,-0.4,-0.15));
#9080=CARTESIAN_POINT('',(0.0866025403784439,-0.4,-0.15));
#9081=CARTESIAN_POINT('',(-0.0866025403784438,-0.64,-0.15));
#9082=CARTESIAN_POINT('',(-0.0866025403784438,-0.4,-0.15));
#9083=CARTESIAN_POINT('',(0.0866025403784439,-0.64,-0.15));
#9084=CARTESIAN_POINT('Origin',(-0.173205080756888,-0.4,-2.77555756156289E-17));
#9085=CARTESIAN_POINT('',(-0.173205080756888,-0.4,-2.12115047744981E-17));
#9086=CARTESIAN_POINT('',(-0.0866025403784438,-0.4,-0.15));
#9087=CARTESIAN_POINT('',(-0.173205080756888,-0.64,-2.77555756156289E-17));
#9088=CARTESIAN_POINT('',(-0.173205080756888,-0.4,-2.12115047744981E-17));
#9089=CARTESIAN_POINT('',(-0.0866025403784438,-0.64,-0.15));
#9090=CARTESIAN_POINT('Origin',(-0.0866025403784439,-0.4,0.15));
#9091=CARTESIAN_POINT('',(-0.0866025403784439,-0.4,0.15));
#9092=CARTESIAN_POINT('',(-0.173205080756888,-0.4,-2.12115047744981E-17));
#9093=CARTESIAN_POINT('',(-0.0866025403784439,-0.64,0.15));
#9094=CARTESIAN_POINT('',(-0.0866025403784439,-0.4,0.15));
#9095=CARTESIAN_POINT('',(-0.173205080756888,-0.64,-2.12115047744981E-17));
#9096=CARTESIAN_POINT('Origin',(0.0866025403784439,-0.4,0.15));
#9097=CARTESIAN_POINT('',(0.0866025403784439,-0.4,0.15));
#9098=CARTESIAN_POINT('',(-0.0866025403784439,-0.4,0.15));
#9099=CARTESIAN_POINT('',(0.0866025403784439,-0.64,0.15));
#9100=CARTESIAN_POINT('',(0.0866025403784439,-0.4,0.15));
#9101=CARTESIAN_POINT('',(-0.0866025403784439,-0.64,0.15));
#9102=CARTESIAN_POINT('Origin',(0.173205080756888,-0.4,0.));
#9103=CARTESIAN_POINT('',(0.0866025403784439,-0.4,0.15));
#9104=CARTESIAN_POINT('',(0.0866025403784439,-0.64,0.15));
#9105=CARTESIAN_POINT('Origin',(0.,-0.4,-2.77555756156289E-17));
#9106=CARTESIAN_POINT('Origin',(0.,-0.64,-2.77555756156289E-17));
#9107=CARTESIAN_POINT('Origin',(0.,-1.,0.));
#9108=CARTESIAN_POINT('',(-0.1954,-1.,2.39295984553393E-17));
#9109=CARTESIAN_POINT('Origin',(0.,-1.,0.));
#9110=CARTESIAN_POINT('Origin',(0.3,0.4,0.));
#9111=CARTESIAN_POINT('',(-0.3,0.4,-3.67394039744206E-17));
#9112=CARTESIAN_POINT('Origin',(0.,0.4,0.));
#9113=CARTESIAN_POINT('Origin',(0.,0.375,0.));
#9114=CARTESIAN_POINT('',(-0.35,0.35,-4.28626379701573E-17));
#9115=CARTESIAN_POINT('Origin',(0.,0.35,0.));
#9116=CARTESIAN_POINT('',(-0.325,0.375,-3.9801020972289E-17));
#9117=CARTESIAN_POINT('Origin',(0.,0.19,0.));
#9118=CARTESIAN_POINT('',(-0.35,0.03,-4.28626379701574E-17));
#9119=CARTESIAN_POINT('Origin',(0.,0.03,0.));
#9120=CARTESIAN_POINT('',(-0.35,0.19,-4.28626379701574E-17));
#9121=CARTESIAN_POINT('Origin',(0.,0.0149999999999999,0.));
#9122=CARTESIAN_POINT('',(-0.32,-3.29597460435593E-17,-3.91886975727153E-17));
#9123=CARTESIAN_POINT('Origin',(0.,0.,0.));
#9124=CARTESIAN_POINT('',(-0.335,0.0149999999999999,-4.10256677714363E-17));
#9125=CARTESIAN_POINT('Origin',(0.22,0.,0.));
#9126=CARTESIAN_POINT('',(-0.22,-6.93889390390723E-18,-2.69422295812418E-17));
#9127=CARTESIAN_POINT('Origin',(0.,0.,0.));
#9128=CARTESIAN_POINT('Origin',(0.,-0.02,0.));
#9129=CARTESIAN_POINT('',(-0.1954,-0.0492,2.39295984553393E-17));
#9130=CARTESIAN_POINT('Origin',(0.,-0.0492,0.));
#9131=CARTESIAN_POINT('',(-0.21,-0.02,-2.57175827820944E-17));
#9132=CARTESIAN_POINT('Origin',(0.,-0.8,0.));
#9133=CARTESIAN_POINT('',(-0.1954,-0.8,-2.39295984553393E-17));
#9134=CARTESIAN_POINT('',(0.,0.,0.));
#9135=CARTESIAN_POINT('',(0.,0.,0.));
#9136=CARTESIAN_POINT('',(0.,0.,0.));
#9137=CARTESIAN_POINT('',(0.,0.,0.));
#9138=CARTESIAN_POINT('',(0.,-1.,12.));
#9139=CARTESIAN_POINT('',(0.,1.,12.));
#9140=CARTESIAN_POINT('',(1.90918830920368,-2.3,13.9091883092037));
#9141=CARTESIAN_POINT('',(-1.90918830920368,-2.3,13.9091883092037));
#9142=CARTESIAN_POINT('',(-1.90918830920368,-2.3,10.0908116907963));
#9143=CARTESIAN_POINT('',(1.90918830920368,-2.3,10.0908116907963));
#9144=CARTESIAN_POINT('',(1.90918830920368,2.3,13.9091883092037));
#9145=CARTESIAN_POINT('',(-1.90918830920368,2.3,13.9091883092037));
#9146=CARTESIAN_POINT('',(-1.90918830920368,2.3,10.0908116907963));
#9147=CARTESIAN_POINT('',(1.90918830920368,2.3,10.0908116907963));
#9148=CARTESIAN_POINT('',(0.,0.,0.));
#9149=CARTESIAN_POINT('',(0.,0.,0.));
#9150=CARTESIAN_POINT('Origin',(0.,0.,4.48));
#9151=CARTESIAN_POINT('',(-1.3,-1.59204083889156E-16,4.48));
#9152=CARTESIAN_POINT('Origin',(0.,0.,4.48));
#9153=CARTESIAN_POINT('',(-0.8,-9.79717439317883E-17,4.48));
#9154=CARTESIAN_POINT('Origin',(0.,0.,4.48));
#9155=CARTESIAN_POINT('Origin',(0.,0.,3.88));
#9156=CARTESIAN_POINT('',(-1.3,-1.59204083889156E-16,3.88));
#9157=CARTESIAN_POINT('Origin',(0.,0.,3.88));
#9158=CARTESIAN_POINT('',(-0.8,9.79717439317883E-17,3.88));
#9159=CARTESIAN_POINT('Origin',(0.,0.,3.88));
#9160=CARTESIAN_POINT('Origin',(0.,0.,3.88));
#9161=CARTESIAN_POINT('',(-1.3,-1.59204083889156E-16,3.88));
#9162=CARTESIAN_POINT('Origin',(0.,0.,3.));
#9163=CARTESIAN_POINT('',(-0.8,-9.79717439317883E-17,3.5));
#9164=CARTESIAN_POINT('',(-0.8,-9.79717439317883E-17,3.));
#9165=CARTESIAN_POINT('',(0.,-0.8,3.5));
#9166=CARTESIAN_POINT('Origin',(0.,0.,3.5));
#9167=CARTESIAN_POINT('',(0.,0.8,3.5));
#9168=CARTESIAN_POINT('Origin',(0.,0.,3.5));
#9169=CARTESIAN_POINT('Origin',(0.,0.,3.5));
#9170=CARTESIAN_POINT('Origin',(0.,0.,3.));
#9171=CARTESIAN_POINT('',(-0.8,-9.79717439317883E-17,6.5));
#9172=CARTESIAN_POINT('Origin',(0.,0.,6.5));
#9173=CARTESIAN_POINT('',(-0.8,-9.79717439317883E-17,3.));
#9174=CARTESIAN_POINT('Origin',(0.,0.,6.5));
#9175=CARTESIAN_POINT('Origin',(-1.,-0.8,3.5));
#9176=CARTESIAN_POINT('',(1.,-0.8,3.5));
#9177=CARTESIAN_POINT('',(1.,-0.8,3.5));
#9178=CARTESIAN_POINT('',(1.,0.8,3.5));
#9179=CARTESIAN_POINT('',(1.,-0.8,3.5));
#9180=CARTESIAN_POINT('',(1.,0.8,3.5));
#9181=CARTESIAN_POINT('Origin',(-1.,-0.8,3.5));
#9182=CARTESIAN_POINT('',(-1.,0.8,3.5));
#9183=CARTESIAN_POINT('',(1.,0.8,3.5));
#9184=CARTESIAN_POINT('',(-1.,-0.8,3.5));
#9185=CARTESIAN_POINT('',(-1.,-0.8,3.5));
#9186=CARTESIAN_POINT('',(1.,-0.8,3.5));
#9187=CARTESIAN_POINT('Origin',(-1.,-0.8,0.));
#9188=CARTESIAN_POINT('',(-1.,-0.8,1.80277563773199));
#9189=CARTESIAN_POINT('',(-1.,0.8,1.80277563773199));
#9190=CARTESIAN_POINT('',(-1.,-0.8,1.80277563773199));
#9191=CARTESIAN_POINT('',(-1.,-0.8,3.5));
#9192=CARTESIAN_POINT('',(-1.,0.8,3.5));
#9193=CARTESIAN_POINT('Origin',(1.,-0.8,0.));
#9194=CARTESIAN_POINT('',(0.,0.8,0.));
#9195=CARTESIAN_POINT('',(0.,-0.8,0.));
#9196=CARTESIAN_POINT('',(0.,-0.8,0.));
#9197=CARTESIAN_POINT('',(1.,0.8,0.));
#9198=CARTESIAN_POINT('',(-1.,0.8,0.));
#9199=CARTESIAN_POINT('',(1.,-0.8,0.));
#9200=CARTESIAN_POINT('',(1.,-0.8,0.));
#9201=CARTESIAN_POINT('',(-1.,-0.8,0.));
#9202=CARTESIAN_POINT('Origin',(2.,0.8,0.));
#9203=CARTESIAN_POINT('',(1.,0.8,0.));
#9204=CARTESIAN_POINT('',(4.,0.8,0.));
#9205=CARTESIAN_POINT('Origin',(2.,0.8,0.));
#9206=CARTESIAN_POINT('',(5.5,0.8,0.));
#9207=CARTESIAN_POINT('',(4.,0.8,0.));
#9208=CARTESIAN_POINT('Origin',(2.,0.8,0.));
#9209=CARTESIAN_POINT('Origin',(2.,-0.8,0.));
#9210=CARTESIAN_POINT('',(4.,-0.8,0.));
#9211=CARTESIAN_POINT('Origin',(2.,-0.8,0.));
#9212=CARTESIAN_POINT('',(4.,-0.8,0.));
#9213=CARTESIAN_POINT('Origin',(2.,-0.8,0.));
#9214=CARTESIAN_POINT('',(1.,-0.8,0.));
#9215=CARTESIAN_POINT('',(5.5,-0.8,0.));
#9216=CARTESIAN_POINT('Origin',(2.,-0.8,0.));
#9217=CARTESIAN_POINT('',(4.,-0.8,0.));
#9218=CARTESIAN_POINT('Origin',(1.,-0.9,0.));
#9219=CARTESIAN_POINT('Origin',(6.,-0.9,0.));
#9220=CARTESIAN_POINT('',(5.5,-0.8,0.));
#9221=CARTESIAN_POINT('Origin',(2.,-0.8,0.));
#9222=CARTESIAN_POINT('',(0.,0.,0.));
#9223=CARTESIAN_POINT('Origin',(0.,0.,5.5));
#9224=CARTESIAN_POINT('',(-0.81,-9.91963907309356E-17,5.7));
#9225=CARTESIAN_POINT('Origin',(0.,0.,5.7));
#9226=CARTESIAN_POINT('',(-0.81,-9.91963907309356E-17,5.5));
#9227=CARTESIAN_POINT('',(-0.81,-9.91963907309356E-17,5.5));
#9228=CARTESIAN_POINT('Origin',(0.,0.,5.5));
#9229=CARTESIAN_POINT('Origin',(0.,0.,5.5));
#9230=CARTESIAN_POINT('',(-1.5,-1.83697019872103E-16,5.7));
#9231=CARTESIAN_POINT('Origin',(0.,0.,5.7));
#9232=CARTESIAN_POINT('',(-1.5,-1.83697019872103E-16,5.5));
#9233=CARTESIAN_POINT('',(-1.5,-1.83697019872103E-16,5.5));
#9234=CARTESIAN_POINT('Origin',(0.,0.,5.5));
#9235=CARTESIAN_POINT('Origin',(0.,0.,5.7));
#9236=CARTESIAN_POINT('Origin',(0.,0.,5.5));
#9237=CARTESIAN_POINT('',(0.,0.,0.));
#9238=CARTESIAN_POINT('Origin',(0.,0.,5.6));
#9239=CARTESIAN_POINT('',(-0.7,-8.57252759403147E-17,5.7));
#9240=CARTESIAN_POINT('Origin',(0.,0.,5.7));
#9241=CARTESIAN_POINT('',(-0.7,8.57252759403147E-17,6.5));
#9242=CARTESIAN_POINT('',(-0.7,-8.57252759403147E-17,5.6));
#9243=CARTESIAN_POINT('Origin',(0.,0.,6.5));
#9244=CARTESIAN_POINT('Origin',(-0.692820323027552,-1.2,5.7));
#9245=CARTESIAN_POINT('',(-0.692820323027552,-1.2,5.7));
#9246=CARTESIAN_POINT('',(0.692820323027551,-1.2,5.7));
#9247=CARTESIAN_POINT('',(-0.692820323027552,-1.2,5.7));
#9248=CARTESIAN_POINT('',(0.692820323027551,-1.2,6.5));
#9249=CARTESIAN_POINT('',(0.692820323027551,-1.2,5.7));
#9250=CARTESIAN_POINT('',(-0.692820323027552,-1.2,6.5));
#9251=CARTESIAN_POINT('',(-0.692820323027552,-1.2,6.5));
#9252=CARTESIAN_POINT('',(-0.692820323027552,-1.2,5.7));
#9253=CARTESIAN_POINT('Origin',(-1.3856406460551,1.69692038195985E-16,5.7));
#9254=CARTESIAN_POINT('',(-1.3856406460551,1.69692038195985E-16,5.7));
#9255=CARTESIAN_POINT('',(-1.3856406460551,1.69692038195985E-16,5.7));
#9256=CARTESIAN_POINT('',(-1.3856406460551,2.22044604925031E-16,6.5));
#9257=CARTESIAN_POINT('',(-1.3856406460551,1.69692038195985E-16,6.5));
#9258=CARTESIAN_POINT('',(-1.3856406460551,1.69692038195985E-16,5.7));
#9259=CARTESIAN_POINT('Origin',(-0.692820323027551,1.2,5.7));
#9260=CARTESIAN_POINT('',(-0.692820323027551,1.2,5.7));
#9261=CARTESIAN_POINT('',(-0.692820323027551,1.2,5.7));
#9262=CARTESIAN_POINT('',(-0.692820323027551,1.2,6.5));
#9263=CARTESIAN_POINT('',(-0.692820323027551,1.2,6.5));
#9264=CARTESIAN_POINT('',(-0.692820323027551,1.2,5.7));
#9265=CARTESIAN_POINT('Origin',(0.692820323027551,1.2,5.7));
#9266=CARTESIAN_POINT('',(0.692820323027551,1.2,5.7));
#9267=CARTESIAN_POINT('',(0.692820323027551,1.2,5.7));
#9268=CARTESIAN_POINT('',(0.692820323027551,1.2,6.5));
#9269=CARTESIAN_POINT('',(0.692820323027551,1.2,6.5));
#9270=CARTESIAN_POINT('',(0.692820323027551,1.2,5.7));
#9271=CARTESIAN_POINT('Origin',(1.3856406460551,0.,5.7));
#9272=CARTESIAN_POINT('',(1.3856406460551,0.,5.7));
#9273=CARTESIAN_POINT('',(1.3856406460551,0.,5.7));
#9274=CARTESIAN_POINT('',(1.3856406460551,0.,6.5));
#9275=CARTESIAN_POINT('',(1.3856406460551,0.,6.5));
#9276=CARTESIAN_POINT('',(1.3856406460551,0.,5.7));
#9277=CARTESIAN_POINT('Origin',(0.692820323027551,-1.2,5.7));
#9278=CARTESIAN_POINT('',(0.692820323027551,-1.2,5.7));
#9279=CARTESIAN_POINT('',(0.692820323027551,-1.2,6.5));
#9280=CARTESIAN_POINT('Origin',(0.,2.22044604925031E-16,6.5));
#9281=CARTESIAN_POINT('Origin',(0.,2.22044604925031E-16,5.7));
#9282=CARTESIAN_POINT('',(0.,0.,0.));
#9283=CARTESIAN_POINT('',(0.,0.,0.));
#9284=CARTESIAN_POINT('',(0.,0.,0.));
#9285=CARTESIAN_POINT('',(0.,0.,0.));
#9286=CARTESIAN_POINT('',(0.,0.,0.));
#9287=CARTESIAN_POINT('Origin',(0.,-0.9,20.5));
#9288=CARTESIAN_POINT('',(-1.,-0.8,20.5));
#9289=CARTESIAN_POINT('Origin',(0.,-0.8,20.5));
#9290=CARTESIAN_POINT('',(-1.,0.8,20.5));
#9291=CARTESIAN_POINT('',(-1.,-0.9,20.5));
#9292=CARTESIAN_POINT('Origin',(0.,0.8,20.5));
#9293=CARTESIAN_POINT('Origin',(0.,-0.9,24.));
#9294=CARTESIAN_POINT('',(-1.,-0.8,24.));
#9295=CARTESIAN_POINT('Origin',(0.,-0.8,24.));
#9296=CARTESIAN_POINT('',(-1.,0.8,24.));
#9297=CARTESIAN_POINT('',(-1.,-0.9,24.));
#9298=CARTESIAN_POINT('Origin',(0.,0.8,24.));
#9299=CARTESIAN_POINT('Origin',(0.,-0.8,24.));
#9300=CARTESIAN_POINT('',(-0.968245836551854,-0.8,22.25));
#9301=CARTESIAN_POINT('',(-0.968245836551854,0.8,22.25));
#9302=CARTESIAN_POINT('',(-0.968245836551854,-0.8,22.25));
#9303=CARTESIAN_POINT('',(0.968245836551854,-0.8,22.25));
#9304=CARTESIAN_POINT('Origin',(0.,-0.8,24.));
#9305=CARTESIAN_POINT('',(0.968245836551854,0.8,22.25));
#9306=CARTESIAN_POINT('',(0.968245836551854,-0.8,22.25));
#9307=CARTESIAN_POINT('Origin',(0.,0.8,24.));
#9308=CARTESIAN_POINT('Origin',(0.,0.8,20.5));
#9309=CARTESIAN_POINT('Origin',(0.,0.8,20.5));
#9310=CARTESIAN_POINT('Origin',(0.,-0.8,20.5));
#9311=CARTESIAN_POINT('Origin',(0.,-0.8,20.5));
#9312=CARTESIAN_POINT('Origin',(0.,-0.8,20.5));
#9313=CARTESIAN_POINT('',(0.,0.,0.));
#9314=CARTESIAN_POINT('',(0.,0.,0.));
#9315=CARTESIAN_POINT('',(0.,0.,0.));
#9316=CARTESIAN_POINT('',(0.,0.,0.));
#9317=CARTESIAN_POINT('',(0.,0.,0.));
#9318=UNCERTAINTY_MEASURE_WITH_UNIT(LENGTH_MEASURE(0.001),#9392,
'DISTANCE_ACCURACY_VALUE',
'Maximum model space distance between geometric entities at asserted c
onnectivities');
#9319=UNCERTAINTY_MEASURE_WITH_UNIT(LENGTH_MEASURE(0.001),#9392,
'DISTANCE_ACCURACY_VALUE',
'Maximum model space distance between geometric entities at asserted c
onnectivities');
#9320=UNCERTAINTY_MEASURE_WITH_UNIT(LENGTH_MEASURE(0.001),#9392,
'DISTANCE_ACCURACY_VALUE',
'Maximum model space distance between geometric entities at asserted c
onnectivities');
#9321=UNCERTAINTY_MEASURE_WITH_UNIT(LENGTH_MEASURE(0.001),#9392,
'DISTANCE_ACCURACY_VALUE',
'Maximum model space distance between geometric entities at asserted c
onnectivities');
#9322=UNCERTAINTY_MEASURE_WITH_UNIT(LENGTH_MEASURE(0.001),#9392,
'DISTANCE_ACCURACY_VALUE',
'Maximum model space distance between geometric entities at asserted c
onnectivities');
#9323=UNCERTAINTY_MEASURE_WITH_UNIT(LENGTH_MEASURE(0.001),#9392,
'DISTANCE_ACCURACY_VALUE',
'Maximum model space distance between geometric entities at asserted c
onnectivities');
#9324=UNCERTAINTY_MEASURE_WITH_UNIT(LENGTH_MEASURE(0.001),#9392,
'DISTANCE_ACCURACY_VALUE',
'Maximum model space distance between geometric entities at asserted c
onnectivities');
#9325=UNCERTAINTY_MEASURE_WITH_UNIT(LENGTH_MEASURE(0.001),#9392,
'DISTANCE_ACCURACY_VALUE',
'Maximum model space distance between geometric entities at asserted c
onnectivities');
#9326=UNCERTAINTY_MEASURE_WITH_UNIT(LENGTH_MEASURE(0.001),#9392,
'DISTANCE_ACCURACY_VALUE',
'Maximum model space distance between geometric entities at asserted c
onnectivities');
#9327=UNCERTAINTY_MEASURE_WITH_UNIT(LENGTH_MEASURE(0.001),#9392,
'DISTANCE_ACCURACY_VALUE',
'Maximum model space distance between geometric entities at asserted c
onnectivities');
#9328=UNCERTAINTY_MEASURE_WITH_UNIT(LENGTH_MEASURE(0.001),#9392,
'DISTANCE_ACCURACY_VALUE',
'Maximum model space distance between geometric entities at asserted c
onnectivities');
#9329=UNCERTAINTY_MEASURE_WITH_UNIT(LENGTH_MEASURE(0.001),#9392,
'DISTANCE_ACCURACY_VALUE',
'Maximum model space distance between geometric entities at asserted c
onnectivities');
#9330=UNCERTAINTY_MEASURE_WITH_UNIT(LENGTH_MEASURE(0.001),#9392,
'DISTANCE_ACCURACY_VALUE',
'Maximum model space distance between geometric entities at asserted c
onnectivities');
#9331=UNCERTAINTY_MEASURE_WITH_UNIT(LENGTH_MEASURE(0.001),#9392,
'DISTANCE_ACCURACY_VALUE',
'Maximum model space distance between geometric entities at asserted c
onnectivities');
#9332=UNCERTAINTY_MEASURE_WITH_UNIT(LENGTH_MEASURE(0.001),#9392,
'DISTANCE_ACCURACY_VALUE',
'Maximum model space distance between geometric entities at asserted c
onnectivities');
#9333=UNCERTAINTY_MEASURE_WITH_UNIT(LENGTH_MEASURE(0.001),#9392,
'DISTANCE_ACCURACY_VALUE',
'Maximum model space distance between geometric entities at asserted c
onnectivities');
#9334=UNCERTAINTY_MEASURE_WITH_UNIT(LENGTH_MEASURE(0.001),#9392,
'DISTANCE_ACCURACY_VALUE',
'Maximum model space distance between geometric entities at asserted c
onnectivities');
#9335=UNCERTAINTY_MEASURE_WITH_UNIT(LENGTH_MEASURE(0.001),#9392,
'DISTANCE_ACCURACY_VALUE',
'Maximum model space distance between geometric entities at asserted c
onnectivities');
#9336=UNCERTAINTY_MEASURE_WITH_UNIT(LENGTH_MEASURE(0.001),#9392,
'DISTANCE_ACCURACY_VALUE',
'Maximum model space distance between geometric entities at asserted c
onnectivities');
#9337=UNCERTAINTY_MEASURE_WITH_UNIT(LENGTH_MEASURE(0.001),#9392,
'DISTANCE_ACCURACY_VALUE',
'Maximum model space distance between geometric entities at asserted c
onnectivities');
#9338=UNCERTAINTY_MEASURE_WITH_UNIT(LENGTH_MEASURE(0.001),#9392,
'DISTANCE_ACCURACY_VALUE',
'Maximum model space distance between geometric entities at asserted c
onnectivities');
#9339=UNCERTAINTY_MEASURE_WITH_UNIT(LENGTH_MEASURE(0.001),#9392,
'DISTANCE_ACCURACY_VALUE',
'Maximum model space distance between geometric entities at asserted c
onnectivities');
#9340=UNCERTAINTY_MEASURE_WITH_UNIT(LENGTH_MEASURE(0.001),#9392,
'DISTANCE_ACCURACY_VALUE',
'Maximum model space distance between geometric entities at asserted c
onnectivities');
#9341=UNCERTAINTY_MEASURE_WITH_UNIT(LENGTH_MEASURE(0.001),#9392,
'DISTANCE_ACCURACY_VALUE',
'Maximum model space distance between geometric entities at asserted c
onnectivities');
#9342=UNCERTAINTY_MEASURE_WITH_UNIT(LENGTH_MEASURE(0.001),#9392,
'DISTANCE_ACCURACY_VALUE',
'Maximum model space distance between geometric entities at asserted c
onnectivities');
#9343=UNCERTAINTY_MEASURE_WITH_UNIT(LENGTH_MEASURE(0.001),#9392,
'DISTANCE_ACCURACY_VALUE',
'Maximum model space distance between geometric entities at asserted c
onnectivities');
#9344=UNCERTAINTY_MEASURE_WITH_UNIT(LENGTH_MEASURE(0.001),#9392,
'DISTANCE_ACCURACY_VALUE',
'Maximum model space distance between geometric entities at asserted c
onnectivities');
#9345=UNCERTAINTY_MEASURE_WITH_UNIT(LENGTH_MEASURE(0.001),#9392,
'DISTANCE_ACCURACY_VALUE',
'Maximum model space distance between geometric entities at asserted c
onnectivities');
#9346=UNCERTAINTY_MEASURE_WITH_UNIT(LENGTH_MEASURE(0.001),#9392,
'DISTANCE_ACCURACY_VALUE',
'Maximum model space distance between geometric entities at asserted c
onnectivities');
#9347=UNCERTAINTY_MEASURE_WITH_UNIT(LENGTH_MEASURE(0.001),#9392,
'DISTANCE_ACCURACY_VALUE',
'Maximum model space distance between geometric entities at asserted c
onnectivities');
#9348=UNCERTAINTY_MEASURE_WITH_UNIT(LENGTH_MEASURE(0.001),#9392,
'DISTANCE_ACCURACY_VALUE',
'Maximum model space distance between geometric entities at asserted c
onnectivities');
#9349=UNCERTAINTY_MEASURE_WITH_UNIT(LENGTH_MEASURE(0.001),#9392,
'DISTANCE_ACCURACY_VALUE',
'Maximum model space distance between geometric entities at asserted c
onnectivities');
#9350=UNCERTAINTY_MEASURE_WITH_UNIT(LENGTH_MEASURE(0.001),#9392,
'DISTANCE_ACCURACY_VALUE',
'Maximum model space distance between geometric entities at asserted c
onnectivities');
#9351=UNCERTAINTY_MEASURE_WITH_UNIT(LENGTH_MEASURE(0.001),#9392,
'DISTANCE_ACCURACY_VALUE',
'Maximum model space distance between geometric entities at asserted c
onnectivities');
#9352=UNCERTAINTY_MEASURE_WITH_UNIT(LENGTH_MEASURE(0.001),#9392,
'DISTANCE_ACCURACY_VALUE',
'Maximum model space distance between geometric entities at asserted c
onnectivities');
#9353=UNCERTAINTY_MEASURE_WITH_UNIT(LENGTH_MEASURE(0.001),#9392,
'DISTANCE_ACCURACY_VALUE',
'Maximum model space distance between geometric entities at asserted c
onnectivities');
#9354=UNCERTAINTY_MEASURE_WITH_UNIT(LENGTH_MEASURE(0.001),#9392,
'DISTANCE_ACCURACY_VALUE',
'Maximum model space distance between geometric entities at asserted c
onnectivities');
#9355=(
GEOMETRIC_REPRESENTATION_CONTEXT(3)
GLOBAL_UNCERTAINTY_ASSIGNED_CONTEXT((#9318))
GLOBAL_UNIT_ASSIGNED_CONTEXT((#9392,#9394,#9395))
REPRESENTATION_CONTEXT('','3D')
);
#9356=(
GEOMETRIC_REPRESENTATION_CONTEXT(3)
GLOBAL_UNCERTAINTY_ASSIGNED_CONTEXT((#9319))
GLOBAL_UNIT_ASSIGNED_CONTEXT((#9392,#9394,#9395))
REPRESENTATION_CONTEXT('','3D')
);
#9357=(
GEOMETRIC_REPRESENTATION_CONTEXT(3)
GLOBAL_UNCERTAINTY_ASSIGNED_CONTEXT((#9320))
GLOBAL_UNIT_ASSIGNED_CONTEXT((#9392,#9394,#9395))
REPRESENTATION_CONTEXT('','3D')
);
#9358=(
GEOMETRIC_REPRESENTATION_CONTEXT(3)
GLOBAL_UNCERTAINTY_ASSIGNED_CONTEXT((#9321))
GLOBAL_UNIT_ASSIGNED_CONTEXT((#9392,#9394,#9395))
REPRESENTATION_CONTEXT('','3D')
);
#9359=(
GEOMETRIC_REPRESENTATION_CONTEXT(3)
GLOBAL_UNCERTAINTY_ASSIGNED_CONTEXT((#9322))
GLOBAL_UNIT_ASSIGNED_CONTEXT((#9392,#9394,#9395))
REPRESENTATION_CONTEXT('','3D')
);
#9360=(
GEOMETRIC_REPRESENTATION_CONTEXT(3)
GLOBAL_UNCERTAINTY_ASSIGNED_CONTEXT((#9323))
GLOBAL_UNIT_ASSIGNED_CONTEXT((#9392,#9394,#9395))
REPRESENTATION_CONTEXT('','3D')
);
#9361=(
GEOMETRIC_REPRESENTATION_CONTEXT(3)
GLOBAL_UNCERTAINTY_ASSIGNED_CONTEXT((#9324))
GLOBAL_UNIT_ASSIGNED_CONTEXT((#9392,#9394,#9395))
REPRESENTATION_CONTEXT('','3D')
);
#9362=(
GEOMETRIC_REPRESENTATION_CONTEXT(3)
GLOBAL_UNCERTAINTY_ASSIGNED_CONTEXT((#9325))
GLOBAL_UNIT_ASSIGNED_CONTEXT((#9392,#9394,#9395))
REPRESENTATION_CONTEXT('','3D')
);
#9363=(
GEOMETRIC_REPRESENTATION_CONTEXT(3)
GLOBAL_UNCERTAINTY_ASSIGNED_CONTEXT((#9326))
GLOBAL_UNIT_ASSIGNED_CONTEXT((#9392,#9394,#9395))
REPRESENTATION_CONTEXT('','3D')
);
#9364=(
GEOMETRIC_REPRESENTATION_CONTEXT(3)
GLOBAL_UNCERTAINTY_ASSIGNED_CONTEXT((#9327))
GLOBAL_UNIT_ASSIGNED_CONTEXT((#9392,#9394,#9395))
REPRESENTATION_CONTEXT('','3D')
);
#9365=(
GEOMETRIC_REPRESENTATION_CONTEXT(3)
GLOBAL_UNCERTAINTY_ASSIGNED_CONTEXT((#9328))
GLOBAL_UNIT_ASSIGNED_CONTEXT((#9392,#9394,#9395))
REPRESENTATION_CONTEXT('','3D')
);
#9366=(
GEOMETRIC_REPRESENTATION_CONTEXT(3)
GLOBAL_UNCERTAINTY_ASSIGNED_CONTEXT((#9329))
GLOBAL_UNIT_ASSIGNED_CONTEXT((#9392,#9394,#9395))
REPRESENTATION_CONTEXT('','3D')
);
#9367=(
GEOMETRIC_REPRESENTATION_CONTEXT(3)
GLOBAL_UNCERTAINTY_ASSIGNED_CONTEXT((#9330))
GLOBAL_UNIT_ASSIGNED_CONTEXT((#9392,#9394,#9395))
REPRESENTATION_CONTEXT('','3D')
);
#9368=(
GEOMETRIC_REPRESENTATION_CONTEXT(3)
GLOBAL_UNCERTAINTY_ASSIGNED_CONTEXT((#9331))
GLOBAL_UNIT_ASSIGNED_CONTEXT((#9392,#9394,#9395))
REPRESENTATION_CONTEXT('','3D')
);
#9369=(
GEOMETRIC_REPRESENTATION_CONTEXT(3)
GLOBAL_UNCERTAINTY_ASSIGNED_CONTEXT((#9332))
GLOBAL_UNIT_ASSIGNED_CONTEXT((#9392,#9394,#9395))
REPRESENTATION_CONTEXT('','3D')
);
#9370=(
GEOMETRIC_REPRESENTATION_CONTEXT(3)
GLOBAL_UNCERTAINTY_ASSIGNED_CONTEXT((#9333))
GLOBAL_UNIT_ASSIGNED_CONTEXT((#9392,#9394,#9395))
REPRESENTATION_CONTEXT('','3D')
);
#9371=(
GEOMETRIC_REPRESENTATION_CONTEXT(3)
GLOBAL_UNCERTAINTY_ASSIGNED_CONTEXT((#9334))
GLOBAL_UNIT_ASSIGNED_CONTEXT((#9392,#9394,#9395))
REPRESENTATION_CONTEXT('','3D')
);
#9372=(
GEOMETRIC_REPRESENTATION_CONTEXT(3)
GLOBAL_UNCERTAINTY_ASSIGNED_CONTEXT((#9335))
GLOBAL_UNIT_ASSIGNED_CONTEXT((#9392,#9394,#9395))
REPRESENTATION_CONTEXT('','3D')
);
#9373=(
GEOMETRIC_REPRESENTATION_CONTEXT(3)
GLOBAL_UNCERTAINTY_ASSIGNED_CONTEXT((#9336))
GLOBAL_UNIT_ASSIGNED_CONTEXT((#9392,#9394,#9395))
REPRESENTATION_CONTEXT('','3D')
);
#9374=(
GEOMETRIC_REPRESENTATION_CONTEXT(3)
GLOBAL_UNCERTAINTY_ASSIGNED_CONTEXT((#9337))
GLOBAL_UNIT_ASSIGNED_CONTEXT((#9392,#9394,#9395))
REPRESENTATION_CONTEXT('','3D')
);
#9375=(
GEOMETRIC_REPRESENTATION_CONTEXT(3)
GLOBAL_UNCERTAINTY_ASSIGNED_CONTEXT((#9338))
GLOBAL_UNIT_ASSIGNED_CONTEXT((#9392,#9394,#9395))
REPRESENTATION_CONTEXT('','3D')
);
#9376=(
GEOMETRIC_REPRESENTATION_CONTEXT(3)
GLOBAL_UNCERTAINTY_ASSIGNED_CONTEXT((#9339))
GLOBAL_UNIT_ASSIGNED_CONTEXT((#9392,#9394,#9395))
REPRESENTATION_CONTEXT('','3D')
);
#9377=(
GEOMETRIC_REPRESENTATION_CONTEXT(3)
GLOBAL_UNCERTAINTY_ASSIGNED_CONTEXT((#9340))
GLOBAL_UNIT_ASSIGNED_CONTEXT((#9392,#9394,#9395))
REPRESENTATION_CONTEXT('','3D')
);
#9378=(
GEOMETRIC_REPRESENTATION_CONTEXT(3)
GLOBAL_UNCERTAINTY_ASSIGNED_CONTEXT((#9341))
GLOBAL_UNIT_ASSIGNED_CONTEXT((#9392,#9394,#9395))
REPRESENTATION_CONTEXT('','3D')
);
#9379=(
GEOMETRIC_REPRESENTATION_CONTEXT(3)
GLOBAL_UNCERTAINTY_ASSIGNED_CONTEXT((#9342))
GLOBAL_UNIT_ASSIGNED_CONTEXT((#9392,#9394,#9395))
REPRESENTATION_CONTEXT('','3D')
);
#9380=(
GEOMETRIC_REPRESENTATION_CONTEXT(3)
GLOBAL_UNCERTAINTY_ASSIGNED_CONTEXT((#9343))
GLOBAL_UNIT_ASSIGNED_CONTEXT((#9392,#9394,#9395))
REPRESENTATION_CONTEXT('','3D')
);
#9381=(
GEOMETRIC_REPRESENTATION_CONTEXT(3)
GLOBAL_UNCERTAINTY_ASSIGNED_CONTEXT((#9344))
GLOBAL_UNIT_ASSIGNED_CONTEXT((#9392,#9394,#9395))
REPRESENTATION_CONTEXT('','3D')
);
#9382=(
GEOMETRIC_REPRESENTATION_CONTEXT(3)
GLOBAL_UNCERTAINTY_ASSIGNED_CONTEXT((#9345))
GLOBAL_UNIT_ASSIGNED_CONTEXT((#9392,#9394,#9395))
REPRESENTATION_CONTEXT('','3D')
);
#9383=(
GEOMETRIC_REPRESENTATION_CONTEXT(3)
GLOBAL_UNCERTAINTY_ASSIGNED_CONTEXT((#9346))
GLOBAL_UNIT_ASSIGNED_CONTEXT((#9392,#9394,#9395))
REPRESENTATION_CONTEXT('','3D')
);
#9384=(
GEOMETRIC_REPRESENTATION_CONTEXT(3)
GLOBAL_UNCERTAINTY_ASSIGNED_CONTEXT((#9347))
GLOBAL_UNIT_ASSIGNED_CONTEXT((#9392,#9394,#9395))
REPRESENTATION_CONTEXT('','3D')
);
#9385=(
GEOMETRIC_REPRESENTATION_CONTEXT(3)
GLOBAL_UNCERTAINTY_ASSIGNED_CONTEXT((#9348))
GLOBAL_UNIT_ASSIGNED_CONTEXT((#9392,#9394,#9395))
REPRESENTATION_CONTEXT('','3D')
);
#9386=(
GEOMETRIC_REPRESENTATION_CONTEXT(3)
GLOBAL_UNCERTAINTY_ASSIGNED_CONTEXT((#9349))
GLOBAL_UNIT_ASSIGNED_CONTEXT((#9392,#9394,#9395))
REPRESENTATION_CONTEXT('','3D')
);
#9387=(
GEOMETRIC_REPRESENTATION_CONTEXT(3)
GLOBAL_UNCERTAINTY_ASSIGNED_CONTEXT((#9350))
GLOBAL_UNIT_ASSIGNED_CONTEXT((#9392,#9394,#9395))
REPRESENTATION_CONTEXT('','3D')
);
#9388=(
GEOMETRIC_REPRESENTATION_CONTEXT(3)
GLOBAL_UNCERTAINTY_ASSIGNED_CONTEXT((#9351))
GLOBAL_UNIT_ASSIGNED_CONTEXT((#9392,#9394,#9395))
REPRESENTATION_CONTEXT('','3D')
);
#9389=(
GEOMETRIC_REPRESENTATION_CONTEXT(3)
GLOBAL_UNCERTAINTY_ASSIGNED_CONTEXT((#9352))
GLOBAL_UNIT_ASSIGNED_CONTEXT((#9392,#9394,#9395))
REPRESENTATION_CONTEXT('','3D')
);
#9390=(
GEOMETRIC_REPRESENTATION_CONTEXT(3)
GLOBAL_UNCERTAINTY_ASSIGNED_CONTEXT((#9353))
GLOBAL_UNIT_ASSIGNED_CONTEXT((#9392,#9394,#9395))
REPRESENTATION_CONTEXT('','3D')
);
#9391=(
GEOMETRIC_REPRESENTATION_CONTEXT(3)
GLOBAL_UNCERTAINTY_ASSIGNED_CONTEXT((#9354))
GLOBAL_UNIT_ASSIGNED_CONTEXT((#9392,#9394,#9395))
REPRESENTATION_CONTEXT('','3D')
);
#9392=(
LENGTH_UNIT()
NAMED_UNIT(*)
SI_UNIT(.CENTI.,.METRE.)
);
#9393=(
LENGTH_UNIT()
NAMED_UNIT(*)
SI_UNIT($,.METRE.)
);
#9394=(
NAMED_UNIT(*)
PLANE_ANGLE_UNIT()
SI_UNIT($,.RADIAN.)
);
#9395=(
NAMED_UNIT(*)
SI_UNIT($,.STERADIAN.)
SOLID_ANGLE_UNIT()
);
#9396=SHAPE_DEFINITION_REPRESENTATION(#9432,#9520);
#9397=SHAPE_DEFINITION_REPRESENTATION(#9433,#9521);
#9398=SHAPE_DEFINITION_REPRESENTATION(#9434,#9522);
#9399=SHAPE_DEFINITION_REPRESENTATION(#9435,#9523);
#9400=SHAPE_DEFINITION_REPRESENTATION(#9436,#9524);
#9401=SHAPE_DEFINITION_REPRESENTATION(#9437,#9525);
#9402=SHAPE_DEFINITION_REPRESENTATION(#9438,#9526);
#9403=SHAPE_DEFINITION_REPRESENTATION(#9439,#9527);
#9404=SHAPE_DEFINITION_REPRESENTATION(#9440,#9528);
#9405=SHAPE_DEFINITION_REPRESENTATION(#9441,#9529);
#9406=SHAPE_DEFINITION_REPRESENTATION(#9442,#9530);
#9407=SHAPE_DEFINITION_REPRESENTATION(#9443,#9531);
#9408=SHAPE_DEFINITION_REPRESENTATION(#9444,#9532);
#9409=SHAPE_DEFINITION_REPRESENTATION(#9445,#9533);
#9410=SHAPE_DEFINITION_REPRESENTATION(#9446,#9534);
#9411=SHAPE_DEFINITION_REPRESENTATION(#9447,#9535);
#9412=SHAPE_DEFINITION_REPRESENTATION(#9448,#9536);
#9413=SHAPE_DEFINITION_REPRESENTATION(#9449,#9537);
#9414=SHAPE_DEFINITION_REPRESENTATION(#9475,#9538);
#9415=SHAPE_DEFINITION_REPRESENTATION(#9476,#9539);
#9416=SHAPE_DEFINITION_REPRESENTATION(#9477,#9540);
#9417=SHAPE_DEFINITION_REPRESENTATION(#9478,#9541);
#9418=SHAPE_DEFINITION_REPRESENTATION(#9479,#9542);
#9419=SHAPE_DEFINITION_REPRESENTATION(#9480,#9543);
#9420=SHAPE_DEFINITION_REPRESENTATION(#9481,#9544);
#9421=SHAPE_DEFINITION_REPRESENTATION(#9482,#9545);
#9422=SHAPE_DEFINITION_REPRESENTATION(#9483,#9546);
#9423=SHAPE_DEFINITION_REPRESENTATION(#9484,#9547);
#9424=SHAPE_DEFINITION_REPRESENTATION(#9485,#9548);
#9425=SHAPE_DEFINITION_REPRESENTATION(#9491,#9549);
#9426=SHAPE_DEFINITION_REPRESENTATION(#9506,#9550);
#9427=SHAPE_DEFINITION_REPRESENTATION(#9507,#9551);
#9428=SHAPE_DEFINITION_REPRESENTATION(#9508,#9552);
#9429=SHAPE_DEFINITION_REPRESENTATION(#9509,#9553);
#9430=SHAPE_DEFINITION_REPRESENTATION(#9513,#9554);
#9431=SHAPE_DEFINITION_REPRESENTATION(#9514,#9555);
#9432=PRODUCT_DEFINITION_SHAPE('',$,#9557);
#9433=PRODUCT_DEFINITION_SHAPE('',$,#9558);
#9434=PRODUCT_DEFINITION_SHAPE('',$,#9559);
#9435=PRODUCT_DEFINITION_SHAPE('',$,#9560);
#9436=PRODUCT_DEFINITION_SHAPE('',$,#9561);
#9437=PRODUCT_DEFINITION_SHAPE('',$,#9562);
#9438=PRODUCT_DEFINITION_SHAPE('',$,#9563);
#9439=PRODUCT_DEFINITION_SHAPE('',$,#9564);
#9440=PRODUCT_DEFINITION_SHAPE('',$,#9565);
#9441=PRODUCT_DEFINITION_SHAPE('',$,#9566);
#9442=PRODUCT_DEFINITION_SHAPE('',$,#9567);
#9443=PRODUCT_DEFINITION_SHAPE('',$,#9568);
#9444=PRODUCT_DEFINITION_SHAPE('',$,#9569);
#9445=PRODUCT_DEFINITION_SHAPE('',$,#9570);
#9446=PRODUCT_DEFINITION_SHAPE('',$,#9571);
#9447=PRODUCT_DEFINITION_SHAPE('',$,#9572);
#9448=PRODUCT_DEFINITION_SHAPE('',$,#9573);
#9449=PRODUCT_DEFINITION_SHAPE('',$,#9574);
#9450=PRODUCT_DEFINITION_SHAPE($,$,#203);
#9451=PRODUCT_DEFINITION_SHAPE($,$,#204);
#9452=PRODUCT_DEFINITION_SHAPE($,$,#205);
#9453=PRODUCT_DEFINITION_SHAPE($,$,#206);
#9454=PRODUCT_DEFINITION_SHAPE($,$,#207);
#9455=PRODUCT_DEFINITION_SHAPE($,$,#208);
#9456=PRODUCT_DEFINITION_SHAPE($,$,#209);
#9457=PRODUCT_DEFINITION_SHAPE($,$,#210);
#9458=PRODUCT_DEFINITION_SHAPE($,$,#211);
#9459=PRODUCT_DEFINITION_SHAPE($,$,#212);
#9460=PRODUCT_DEFINITION_SHAPE($,$,#213);
#9461=PRODUCT_DEFINITION_SHAPE($,$,#214);
#9462=PRODUCT_DEFINITION_SHAPE($,$,#215);
#9463=PRODUCT_DEFINITION_SHAPE($,$,#216);
#9464=PRODUCT_DEFINITION_SHAPE($,$,#217);
#9465=PRODUCT_DEFINITION_SHAPE($,$,#218);
#9466=PRODUCT_DEFINITION_SHAPE($,$,#219);
#9467=PRODUCT_DEFINITION_SHAPE($,$,#220);
#9468=PRODUCT_DEFINITION_SHAPE($,$,#221);
#9469=PRODUCT_DEFINITION_SHAPE($,$,#222);
#9470=PRODUCT_DEFINITION_SHAPE($,$,#223);
#9471=PRODUCT_DEFINITION_SHAPE($,$,#224);
#9472=PRODUCT_DEFINITION_SHAPE($,$,#225);
#9473=PRODUCT_DEFINITION_SHAPE($,$,#226);
#9474=PRODUCT_DEFINITION_SHAPE($,$,#227);
#9475=PRODUCT_DEFINITION_SHAPE('',$,#9575);
#9476=PRODUCT_DEFINITION_SHAPE('',$,#9576);
#9477=PRODUCT_DEFINITION_SHAPE('',$,#9577);
#9478=PRODUCT_DEFINITION_SHAPE('',$,#9578);
#9479=PRODUCT_DEFINITION_SHAPE('',$,#9579);
#9480=PRODUCT_DEFINITION_SHAPE('',$,#9580);
#9481=PRODUCT_DEFINITION_SHAPE('',$,#9581);
#9482=PRODUCT_DEFINITION_SHAPE('',$,#9582);
#9483=PRODUCT_DEFINITION_SHAPE('',$,#9583);
#9484=PRODUCT_DEFINITION_SHAPE('',$,#9584);
#9485=PRODUCT_DEFINITION_SHAPE('',$,#9585);
#9486=PRODUCT_DEFINITION_SHAPE($,$,#228);
#9487=PRODUCT_DEFINITION_SHAPE($,$,#229);
#9488=PRODUCT_DEFINITION_SHAPE($,$,#230);
#9489=PRODUCT_DEFINITION_SHAPE($,$,#231);
#9490=PRODUCT_DEFINITION_SHAPE($,$,#232);
#9491=PRODUCT_DEFINITION_SHAPE('',$,#9586);
#9492=PRODUCT_DEFINITION_SHAPE($,$,#233);
#9493=PRODUCT_DEFINITION_SHAPE($,$,#234);
#9494=PRODUCT_DEFINITION_SHAPE($,$,#235);
#9495=PRODUCT_DEFINITION_SHAPE($,$,#236);
#9496=PRODUCT_DEFINITION_SHAPE($,$,#237);
#9497=PRODUCT_DEFINITION_SHAPE($,$,#238);
#9498=PRODUCT_DEFINITION_SHAPE($,$,#239);
#9499=PRODUCT_DEFINITION_SHAPE($,$,#240);
#9500=PRODUCT_DEFINITION_SHAPE($,$,#241);
#9501=PRODUCT_DEFINITION_SHAPE($,$,#242);
#9502=PRODUCT_DEFINITION_SHAPE($,$,#243);
#9503=PRODUCT_DEFINITION_SHAPE($,$,#244);
#9504=PRODUCT_DEFINITION_SHAPE($,$,#245);
#9505=PRODUCT_DEFINITION_SHAPE($,$,#246);
#9506=PRODUCT_DEFINITION_SHAPE('',$,#9587);
#9507=PRODUCT_DEFINITION_SHAPE('',$,#9588);
#9508=PRODUCT_DEFINITION_SHAPE('',$,#9589);
#9509=PRODUCT_DEFINITION_SHAPE('',$,#9590);
#9510=PRODUCT_DEFINITION_SHAPE($,$,#247);
#9511=PRODUCT_DEFINITION_SHAPE($,$,#248);
#9512=PRODUCT_DEFINITION_SHAPE($,$,#249);
#9513=PRODUCT_DEFINITION_SHAPE('',$,#9591);
#9514=PRODUCT_DEFINITION_SHAPE('',$,#9592);
#9515=PRODUCT_DEFINITION_SHAPE($,$,#250);
#9516=PRODUCT_DEFINITION_SHAPE($,$,#251);
#9517=PRODUCT_DEFINITION_SHAPE($,$,#252);
#9518=PRODUCT_DEFINITION_SHAPE($,$,#253);
#9519=PRODUCT_DEFINITION_SHAPE($,$,#254);
#9520=SHAPE_REPRESENTATION('',(#5259,#5925,#5926,#5927,#5928),#9355);
#9521=SHAPE_REPRESENTATION('',(#5260,#5562,#5563,#5564,#5565,#5566,#5567,
#5568,#5569,#5570,#5571,#5572,#5573,#5574,#5575,#5576,#5577,#5578,#5579,
#5580,#5581,#5582,#5583,#5584,#5585,#5586),#9356);
#9522=SHAPE_REPRESENTATION('',(#5261),#9357);
#9523=SHAPE_REPRESENTATION('',(#5321),#9358);
#9524=SHAPE_REPRESENTATION('',(#5381),#9359);
#9525=SHAPE_REPRESENTATION('',(#5397),#9360);
#9526=SHAPE_REPRESENTATION('',(#5406),#9361);
#9527=SHAPE_REPRESENTATION('',(#5420),#9362);
#9528=SHAPE_REPRESENTATION('',(#5429),#9363);
#9529=SHAPE_REPRESENTATION('',(#5438),#9364);
#9530=SHAPE_REPRESENTATION('',(#5447),#9365);
#9531=SHAPE_REPRESENTATION('',(#5456),#9366);
#9532=SHAPE_REPRESENTATION('',(#5465),#9367);
#9533=SHAPE_REPRESENTATION('',(#5474),#9368);
#9534=SHAPE_REPRESENTATION('',(#5483),#9369);
#9535=SHAPE_REPRESENTATION('',(#5511),#9370);
#9536=SHAPE_REPRESENTATION('',(#5520),#9371);
#9537=SHAPE_REPRESENTATION('',(#5536),#9372);
#9538=SHAPE_REPRESENTATION('',(#5587,#5840,#5841,#5842,#5843,#5844,#5845,
#5846,#5847,#5848,#5849,#5850,#5851,#5852,#5853),#9373);
#9539=SHAPE_REPRESENTATION('',(#5588),#9374);
#9540=SHAPE_REPRESENTATION('',(#5623),#9375);
#9541=SHAPE_REPRESENTATION('',(#5632),#9376);
#9542=SHAPE_REPRESENTATION('',(#5657),#9377);
#9543=SHAPE_REPRESENTATION('',(#5682,#5811,#5812,#5813,#5814,#5815),#9378);
#9544=SHAPE_REPRESENTATION('',(#5683),#9379);
#9545=SHAPE_REPRESENTATION('',(#5703),#9380);
#9546=SHAPE_REPRESENTATION('',(#5723),#9381);
#9547=SHAPE_REPRESENTATION('',(#5740),#9382);
#9548=SHAPE_REPRESENTATION('',(#5794),#9383);
#9549=SHAPE_REPRESENTATION('',(#5816),#9384);
#9550=SHAPE_REPRESENTATION('',(#5854,#5905,#5906,#5907),#9385);
#9551=SHAPE_REPRESENTATION('',(#5855),#9386);
#9552=SHAPE_REPRESENTATION('',(#5884),#9387);
#9553=SHAPE_REPRESENTATION('',(#5893),#9388);
#9554=SHAPE_REPRESENTATION('',(#5908,#5924),#9389);
#9555=SHAPE_REPRESENTATION('',(#5909),#9390);
#9556=PRODUCT_DEFINITION_CONTEXT('part definition',#9666,'design');
#9557=PRODUCT_DEFINITION('PAT-067','PAT-067',#9593,
#9556);
#9558=PRODUCT_DEFINITION('Side plates and axles',
'Side plates and axles',#9594,#9556);
#9559=PRODUCT_DEFINITION('Side plate','Side plate',#9595,#9556);
#9560=PRODUCT_DEFINITION('Side plate (1)','Side plate (1)',#9596,#9556);
#9561=PRODUCT_DEFINITION('Hook bridge','Hook bridge',#9597,#9556);
#9562=PRODUCT_DEFINITION('Eye axle sleeve','Eye axle sleeve',#9598,#9556);
#9563=PRODUCT_DEFINITION('Sheave axle','Sheave axle',#9599,#9556);
#9564=PRODUCT_DEFINITION('Axle keeper','Axle keeper',#9600,#9556);
#9565=PRODUCT_DEFINITION('Outer inner-race spacer',
'Outer inner-race spacer',#9601,#9556);
#9566=PRODUCT_DEFINITION('Outer inner-race spacer (1)',
'Outer inner-race spacer (1)',#9602,#9556);
#9567=PRODUCT_DEFINITION('Central inner-race spacer',
'Central inner-race spacer',#9603,#9556);
#9568=PRODUCT_DEFINITION('Hook bushing','Hook bushing',#9604,#9556);
#9569=PRODUCT_DEFINITION('Eye spacer','Eye spacer',#9605,#9556);
#9570=PRODUCT_DEFINITION('Eye spacer (1)','Eye spacer (1)',#9606,#9556);
#9571=PRODUCT_DEFINITION('M8x75 cross bolt','M8x75 cross bolt',#9607,#9556);
#9572=PRODUCT_DEFINITION('Flat Washer - M8','Flat Washer - M8',#9608,#9556);
#9573=PRODUCT_DEFINITION('Hex Nut - M8','Hex Nut - M8',#9609,#9556);
#9574=PRODUCT_DEFINITION('Cap Screw - M8x30','Cap Screw - M8x30',#9610,
#9556);
#9575=PRODUCT_DEFINITION('Rope sheave','Rope sheave',#9611,#9556);
#9576=PRODUCT_DEFINITION('Sheave','Sheave',#9612,#9556);
#9577=PRODUCT_DEFINITION('Outer race spacer','Outer race spacer',#9613,
#9556);
#9578=PRODUCT_DEFINITION('Sheave cap','Sheave cap',#9614,#9556);
#9579=PRODUCT_DEFINITION('Sheave cap (1)','Sheave cap (1)',#9615,#9556);
#9580=PRODUCT_DEFINITION('Sealed Ball Bearing - 20 x 47 x 14 mm',
'Sealed Ball Bearing - 20 x 47 x 14 mm',#9616,#9556);
#9581=PRODUCT_DEFINITION('Inner ring','Inner ring',#9617,#9556);
#9582=PRODUCT_DEFINITION('Outer ring','Outer ring',#9618,#9556);
#9583=PRODUCT_DEFINITION('Balls','Balls',#9619,#9556);
#9584=PRODUCT_DEFINITION('Cage','Cage',#9620,#9556);
#9585=PRODUCT_DEFINITION('Seals 2RS','Seals 2RS',#9621,#9556);
#9586=PRODUCT_DEFINITION('M4x10 Cap Screw','M4x10 Cap Screw',#9622,#9556);
#9587=PRODUCT_DEFINITION('Swivel hook','Swivel hook',#9623,#9556);
#9588=PRODUCT_DEFINITION('Hook','Hook',#9624,#9556);
#9589=PRODUCT_DEFINITION('Swivel thrust washer','Swivel thrust washer',
#9625,#9556);
#9590=PRODUCT_DEFINITION('M16 hook retaining nut',
'M16 hook retaining nut',#9626,#9556);
#9591=PRODUCT_DEFINITION('Lifting eye','Lifting eye',#9627,#9556);
#9592=PRODUCT_DEFINITION('Lifting eye link','Lifting eye link',#9628,#9556);
#9593=PRODUCT_DEFINITION_FORMATION('',$,#9668);
#9594=PRODUCT_DEFINITION_FORMATION('',$,#9669);
#9595=PRODUCT_DEFINITION_FORMATION('',$,#9670);
#9596=PRODUCT_DEFINITION_FORMATION('',$,#9671);
#9597=PRODUCT_DEFINITION_FORMATION('',$,#9672);
#9598=PRODUCT_DEFINITION_FORMATION('',$,#9673);
#9599=PRODUCT_DEFINITION_FORMATION('',$,#9674);
#9600=PRODUCT_DEFINITION_FORMATION('',$,#9675);
#9601=PRODUCT_DEFINITION_FORMATION('',$,#9676);
#9602=PRODUCT_DEFINITION_FORMATION('',$,#9677);
#9603=PRODUCT_DEFINITION_FORMATION('',$,#9678);
#9604=PRODUCT_DEFINITION_FORMATION('',$,#9679);
#9605=PRODUCT_DEFINITION_FORMATION('',$,#9680);
#9606=PRODUCT_DEFINITION_FORMATION('',$,#9681);
#9607=PRODUCT_DEFINITION_FORMATION('',$,#9682);
#9608=PRODUCT_DEFINITION_FORMATION('',$,#9683);
#9609=PRODUCT_DEFINITION_FORMATION('',$,#9684);
#9610=PRODUCT_DEFINITION_FORMATION('',$,#9685);
#9611=PRODUCT_DEFINITION_FORMATION('',$,#9686);
#9612=PRODUCT_DEFINITION_FORMATION('',$,#9687);
#9613=PRODUCT_DEFINITION_FORMATION('',$,#9688);
#9614=PRODUCT_DEFINITION_FORMATION('',$,#9689);
#9615=PRODUCT_DEFINITION_FORMATION('',$,#9690);
#9616=PRODUCT_DEFINITION_FORMATION('',$,#9691);
#9617=PRODUCT_DEFINITION_FORMATION('',$,#9692);
#9618=PRODUCT_DEFINITION_FORMATION('',$,#9693);
#9619=PRODUCT_DEFINITION_FORMATION('',$,#9694);
#9620=PRODUCT_DEFINITION_FORMATION('',$,#9695);
#9621=PRODUCT_DEFINITION_FORMATION('',$,#9696);
#9622=PRODUCT_DEFINITION_FORMATION('',$,#9697);
#9623=PRODUCT_DEFINITION_FORMATION('',$,#9698);
#9624=PRODUCT_DEFINITION_FORMATION('',$,#9699);
#9625=PRODUCT_DEFINITION_FORMATION('',$,#9700);
#9626=PRODUCT_DEFINITION_FORMATION('',$,#9701);
#9627=PRODUCT_DEFINITION_FORMATION('',$,#9702);
#9628=PRODUCT_DEFINITION_FORMATION('',$,#9703);
#9629=PRODUCT_RELATED_PRODUCT_CATEGORY('PAT-067','PAT-067',(#9668));
#9630=PRODUCT_RELATED_PRODUCT_CATEGORY('Side plates and axles',
'Side plates and axles',(#9669));
#9631=PRODUCT_RELATED_PRODUCT_CATEGORY('Side plate','Side plate',(#9670));
#9632=PRODUCT_RELATED_PRODUCT_CATEGORY('Side plate (1)',
'Side plate (1)',(#9671));
#9633=PRODUCT_RELATED_PRODUCT_CATEGORY('Hook bridge','Hook bridge',(#9672));
#9634=PRODUCT_RELATED_PRODUCT_CATEGORY('Eye axle sleeve',
'Eye axle sleeve',(#9673));
#9635=PRODUCT_RELATED_PRODUCT_CATEGORY('Sheave axle','Sheave axle',(#9674));
#9636=PRODUCT_RELATED_PRODUCT_CATEGORY('Axle keeper','Axle keeper',(#9675));
#9637=PRODUCT_RELATED_PRODUCT_CATEGORY('Outer inner-race spacer',
'Outer inner-race spacer',(#9676));
#9638=PRODUCT_RELATED_PRODUCT_CATEGORY('Outer inner-race spacer (1)',
'Outer inner-race spacer (1)',(#9677));
#9639=PRODUCT_RELATED_PRODUCT_CATEGORY('Central inner-race spacer',
'Central inner-race spacer',(#9678));
#9640=PRODUCT_RELATED_PRODUCT_CATEGORY('Hook bushing','Hook bushing',(#9679));
#9641=PRODUCT_RELATED_PRODUCT_CATEGORY('Eye spacer','Eye spacer',(#9680));
#9642=PRODUCT_RELATED_PRODUCT_CATEGORY('Eye spacer (1)',
'Eye spacer (1)',(#9681));
#9643=PRODUCT_RELATED_PRODUCT_CATEGORY('M8x75 cross bolt',
'M8x75 cross bolt',(#9682));
#9644=PRODUCT_RELATED_PRODUCT_CATEGORY('Flat Washer - M8',
'Flat Washer - M8',(#9683));
#9645=PRODUCT_RELATED_PRODUCT_CATEGORY('Hex Nut - M8','Hex Nut - M8',(#9684));
#9646=PRODUCT_RELATED_PRODUCT_CATEGORY('Cap Screw - M8x30',
'Cap Screw - M8x30',(#9685));
#9647=PRODUCT_RELATED_PRODUCT_CATEGORY('Rope sheave','Rope sheave',(#9686));
#9648=PRODUCT_RELATED_PRODUCT_CATEGORY('Sheave','Sheave',(#9687));
#9649=PRODUCT_RELATED_PRODUCT_CATEGORY('Outer race spacer',
'Outer race spacer',(#9688));
#9650=PRODUCT_RELATED_PRODUCT_CATEGORY('Sheave cap','Sheave cap',(#9689));
#9651=PRODUCT_RELATED_PRODUCT_CATEGORY('Sheave cap (1)',
'Sheave cap (1)',(#9690));
#9652=PRODUCT_RELATED_PRODUCT_CATEGORY(
'Sealed Ball Bearing - 20 x 47 x 14 mm',
'Sealed Ball Bearing - 20 x 47 x 14 mm',(#9691));
#9653=PRODUCT_RELATED_PRODUCT_CATEGORY('Inner ring','Inner ring',(#9692));
#9654=PRODUCT_RELATED_PRODUCT_CATEGORY('Outer ring','Outer ring',(#9693));
#9655=PRODUCT_RELATED_PRODUCT_CATEGORY('Balls','Balls',(#9694));
#9656=PRODUCT_RELATED_PRODUCT_CATEGORY('Cage','Cage',(#9695));
#9657=PRODUCT_RELATED_PRODUCT_CATEGORY('Seals 2RS','Seals 2RS',(#9696));
#9658=PRODUCT_RELATED_PRODUCT_CATEGORY('M4x10 Cap Screw',
'M4x10 Cap Screw',(#9697));
#9659=PRODUCT_RELATED_PRODUCT_CATEGORY('Swivel hook','Swivel hook',(#9698));
#9660=PRODUCT_RELATED_PRODUCT_CATEGORY('Hook','Hook',(#9699));
#9661=PRODUCT_RELATED_PRODUCT_CATEGORY('Swivel thrust washer',
'Swivel thrust washer',(#9700));
#9662=PRODUCT_RELATED_PRODUCT_CATEGORY('M16 hook retaining nut',
'M16 hook retaining nut',(#9701));
#9663=PRODUCT_RELATED_PRODUCT_CATEGORY('Lifting eye','Lifting eye',(#9702));
#9664=PRODUCT_RELATED_PRODUCT_CATEGORY('Lifting eye link',
'Lifting eye link',(#9703));
#9665=APPLICATION_PROTOCOL_DEFINITION('international standard',
'automotive_design',2009,#9666);
#9666=APPLICATION_CONTEXT(
'Core Data for Automotive Mechanical Design Process');
#9667=PRODUCT_CONTEXT('part definition',#9666,'mechanical');
#9668=PRODUCT('PAT-067','PAT-067',
'PAT-067',(#9667));
#9669=PRODUCT('Side plates and axles','Side plates and axles',
'Side plates and axles',(#9667));
#9670=PRODUCT('Side plate','Side plate','Side plate',(#9667));
#9671=PRODUCT('Side plate (1)','Side plate (1)','Side plate (1)',(#9667));
#9672=PRODUCT('Hook bridge','Hook bridge','Hook bridge',(#9667));
#9673=PRODUCT('Eye axle sleeve','Eye axle sleeve','Eye axle sleeve',(#9667));
#9674=PRODUCT('Sheave axle','Sheave axle','Sheave axle',(#9667));
#9675=PRODUCT('Axle keeper','Axle keeper','Axle keeper',(#9667));
#9676=PRODUCT('Outer inner-race spacer','Outer inner-race spacer',
'Outer inner-race spacer',(#9667));
#9677=PRODUCT('Outer inner-race spacer (1)','Outer inner-race spacer (1)',
'Outer inner-race spacer (1)',(#9667));
#9678=PRODUCT('Central inner-race spacer','Central inner-race spacer',
'Central inner-race spacer',(#9667));
#9679=PRODUCT('Hook bushing','Hook bushing','Hook bushing',(#9667));
#9680=PRODUCT('Eye spacer','Eye spacer','Eye spacer',(#9667));
#9681=PRODUCT('Eye spacer (1)','Eye spacer (1)','Eye spacer (1)',(#9667));
#9682=PRODUCT('M8x75 cross bolt','M8x75 cross bolt','M8x75 cross bolt',
(#9667));
#9683=PRODUCT('Flat Washer - M8','Flat Washer - M8','Flat Washer - M8',
(#9667));
#9684=PRODUCT('Hex Nut - M8','Hex Nut - M8','Hex Nut - M8',(#9667));
#9685=PRODUCT('Cap Screw - M8x30','Cap Screw - M8x30',
'Cap Screw - M8x30',(#9667));
#9686=PRODUCT('Rope sheave','Rope sheave','Rope sheave',(#9667));
#9687=PRODUCT('Sheave','Sheave','Sheave',(#9667));
#9688=PRODUCT('Outer race spacer','Outer race spacer',
'Outer race spacer',(#9667));
#9689=PRODUCT('Sheave cap','Sheave cap','Sheave cap',(#9667));
#9690=PRODUCT('Sheave cap (1)','Sheave cap (1)','Sheave cap (1)',(#9667));
#9691=PRODUCT('Sealed Ball Bearing - 20 x 47 x 14 mm',
'Sealed Ball Bearing - 20 x 47 x 14 mm',
'Sealed Ball Bearing - 20 x 47 x 14 mm',(#9667));
#9692=PRODUCT('Inner ring','Inner ring','Inner ring',(#9667));
#9693=PRODUCT('Outer ring','Outer ring','Outer ring',(#9667));
#9694=PRODUCT('Balls','Balls','Balls',(#9667));
#9695=PRODUCT('Cage','Cage','Cage',(#9667));
#9696=PRODUCT('Seals 2RS','Seals 2RS','Seals 2RS',(#9667));
#9697=PRODUCT('M4x10 Cap Screw','M4x10 Cap Screw','M4x10 Cap Screw',(#9667));
#9698=PRODUCT('Swivel hook','Swivel hook','Swivel hook',(#9667));
#9699=PRODUCT('Hook','Hook','Hook',(#9667));
#9700=PRODUCT('Swivel thrust washer','Swivel thrust washer',
'Swivel thrust washer',(#9667));
#9701=PRODUCT('M16 hook retaining nut','M16 hook retaining nut',
'M16 hook retaining nut',(#9667));
#9702=PRODUCT('Lifting eye','Lifting eye','Lifting eye',(#9667));
#9703=PRODUCT('Lifting eye link','Lifting eye link','Lifting eye link',
(#9667));
#9704=PRESENTATION_STYLE_ASSIGNMENT((#9708));
#9705=PRESENTATION_STYLE_ASSIGNMENT((#9709));
#9706=PRESENTATION_STYLE_ASSIGNMENT((#9710));
#9707=PRESENTATION_STYLE_ASSIGNMENT((#9711));
#9708=SURFACE_STYLE_USAGE(.BOTH.,#9712);
#9709=SURFACE_STYLE_USAGE(.BOTH.,#9713);
#9710=SURFACE_STYLE_USAGE(.BOTH.,#9714);
#9711=SURFACE_STYLE_USAGE(.BOTH.,#9715);
#9712=SURFACE_SIDE_STYLE('',(#9716));
#9713=SURFACE_SIDE_STYLE('',(#9717));
#9714=SURFACE_SIDE_STYLE('',(#9718));
#9715=SURFACE_SIDE_STYLE('',(#9719));
#9716=SURFACE_STYLE_FILL_AREA(#9720);
#9717=SURFACE_STYLE_FILL_AREA(#9721);
#9718=SURFACE_STYLE_FILL_AREA(#9722);
#9719=SURFACE_STYLE_FILL_AREA(#9723);
#9720=FILL_AREA_STYLE('Steel - Satin',(#9724));
#9721=FILL_AREA_STYLE('CAD Library Painted - Engineering blue',(#9725));
#9722=FILL_AREA_STYLE('CAD Library Painted - Steel gray',(#9726));
#9723=FILL_AREA_STYLE('CAD Library Painted - Graphite',(#9727));
#9724=FILL_AREA_STYLE_COLOUR('Steel - Satin',#9728);
#9725=FILL_AREA_STYLE_COLOUR('CAD Library Painted - Engineering blue',#9729);
#9726=FILL_AREA_STYLE_COLOUR('CAD Library Painted - Steel gray',#9730);
#9727=FILL_AREA_STYLE_COLOUR('CAD Library Painted - Graphite',#9731);
#9728=COLOUR_RGB('Steel - Satin',0.627450980392157,0.627450980392157,0.627450980392157);
#9729=COLOUR_RGB('CAD Library Painted - Engineering blue',0.12156862745098,
0.356862745098039,0.6);
#9730=COLOUR_RGB('CAD Library Painted - Steel gray',0.592156862745098,0.631372549019608,
0.67843137254902);
#9731=COLOUR_RGB('CAD Library Painted - Graphite',0.168627450980392,0.192156862745098,
0.231372549019608);
#9732=COLOUR_RGB('Dark Blue',0.08,0.2,0.34);
#9733=FILL_AREA_STYLE_COLOUR('',#9732);
#9734=FILL_AREA_STYLE('',(#9733));
#9735=SURFACE_STYLE_FILL_AREA(#9734);
#9736=SURFACE_SIDE_STYLE('',(#9735));
#9737=SURFACE_STYLE_USAGE(.BOTH.,#9736);
#9738=PRESENTATION_STYLE_ASSIGNMENT((#9737));
#9739=COLOUR_RGB('Light Blue',0.38,0.62,0.78);
#9740=FILL_AREA_STYLE_COLOUR('',#9739);
#9741=FILL_AREA_STYLE('',(#9740));
#9742=SURFACE_STYLE_FILL_AREA(#9741);
#9743=SURFACE_SIDE_STYLE('',(#9742));
#9744=SURFACE_STYLE_USAGE(.BOTH.,#9743);
#9745=PRESENTATION_STYLE_ASSIGNMENT((#9744));
#9746=COLOUR_RGB('Sky Blue',0.24,0.69,0.87);
#9747=FILL_AREA_STYLE_COLOUR('',#9746);
#9748=FILL_AREA_STYLE('',(#9747));
#9749=SURFACE_STYLE_FILL_AREA(#9748);
#9750=SURFACE_SIDE_STYLE('',(#9749));
#9751=SURFACE_STYLE_USAGE(.BOTH.,#9750);
#9752=PRESENTATION_STYLE_ASSIGNMENT((#9751));
#9753=COLOUR_RGB('Grey',0.48,0.52,0.57);
#9754=FILL_AREA_STYLE_COLOUR('',#9753);
#9755=FILL_AREA_STYLE('',(#9754));
#9756=SURFACE_STYLE_FILL_AREA(#9755);
#9757=SURFACE_SIDE_STYLE('',(#9756));
#9758=SURFACE_STYLE_USAGE(.BOTH.,#9757);
#9759=PRESENTATION_STYLE_ASSIGNMENT((#9758));
#9760=COLOUR_RGB('Black',0.12,0.14,0.17);
#9761=FILL_AREA_STYLE_COLOUR('',#9760);
#9762=FILL_AREA_STYLE('',(#9761));
#9763=SURFACE_STYLE_FILL_AREA(#9762);
#9764=SURFACE_SIDE_STYLE('',(#9763));
#9765=SURFACE_STYLE_USAGE(.BOTH.,#9764);
#9766=PRESENTATION_STYLE_ASSIGNMENT((#9765));
#9767=COLOUR_RGB('Off White',0.89,0.88,0.83);
#9768=FILL_AREA_STYLE_COLOUR('',#9767);
#9769=FILL_AREA_STYLE('',(#9768));
#9770=SURFACE_STYLE_FILL_AREA(#9769);
#9771=SURFACE_SIDE_STYLE('',(#9770));
#9772=SURFACE_STYLE_USAGE(.BOTH.,#9771);
#9773=PRESENTATION_STYLE_ASSIGNMENT((#9772));
ENDSEC;
END-ISO-10303-21;
